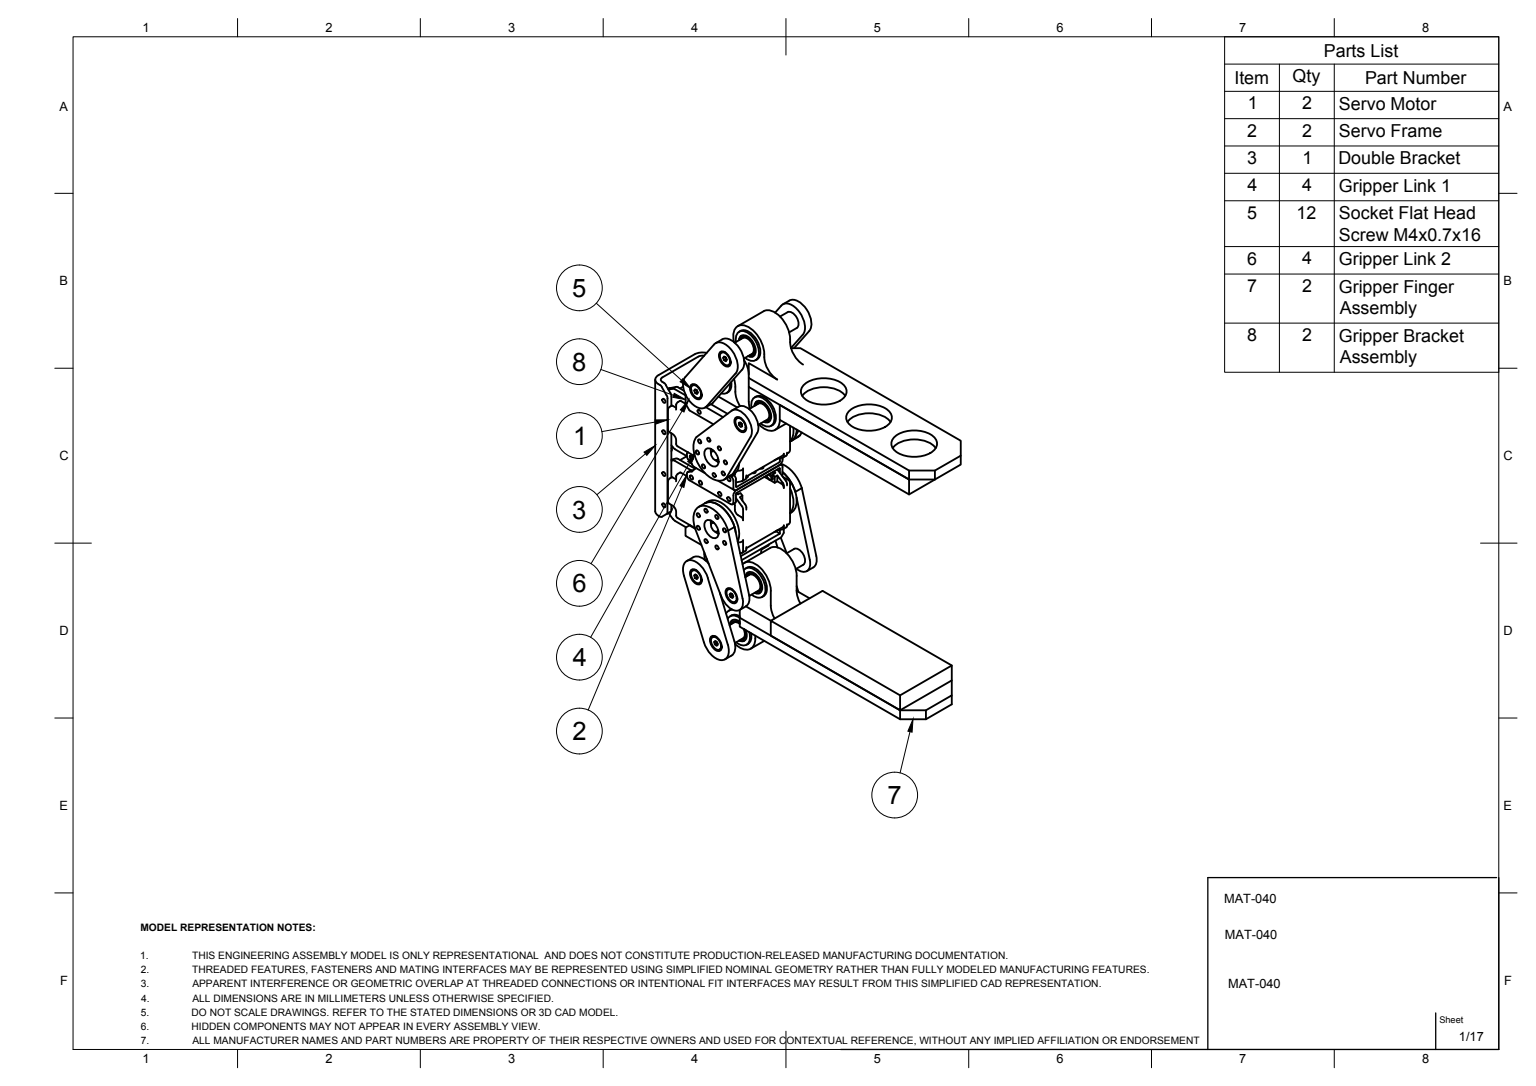
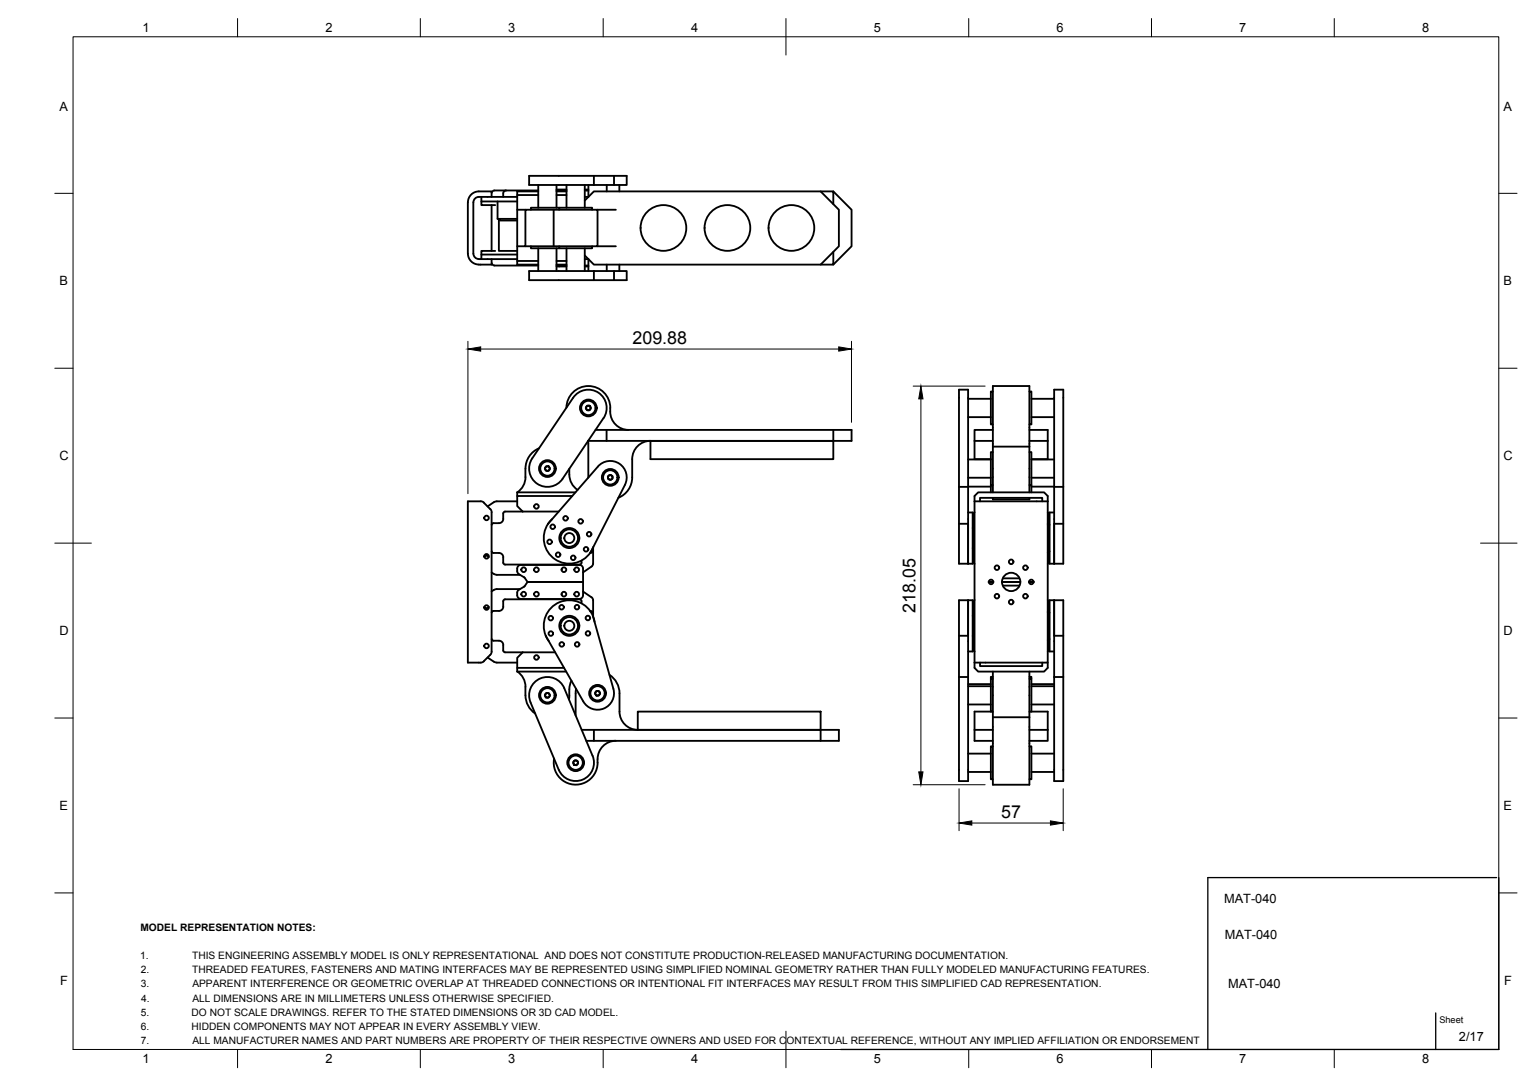
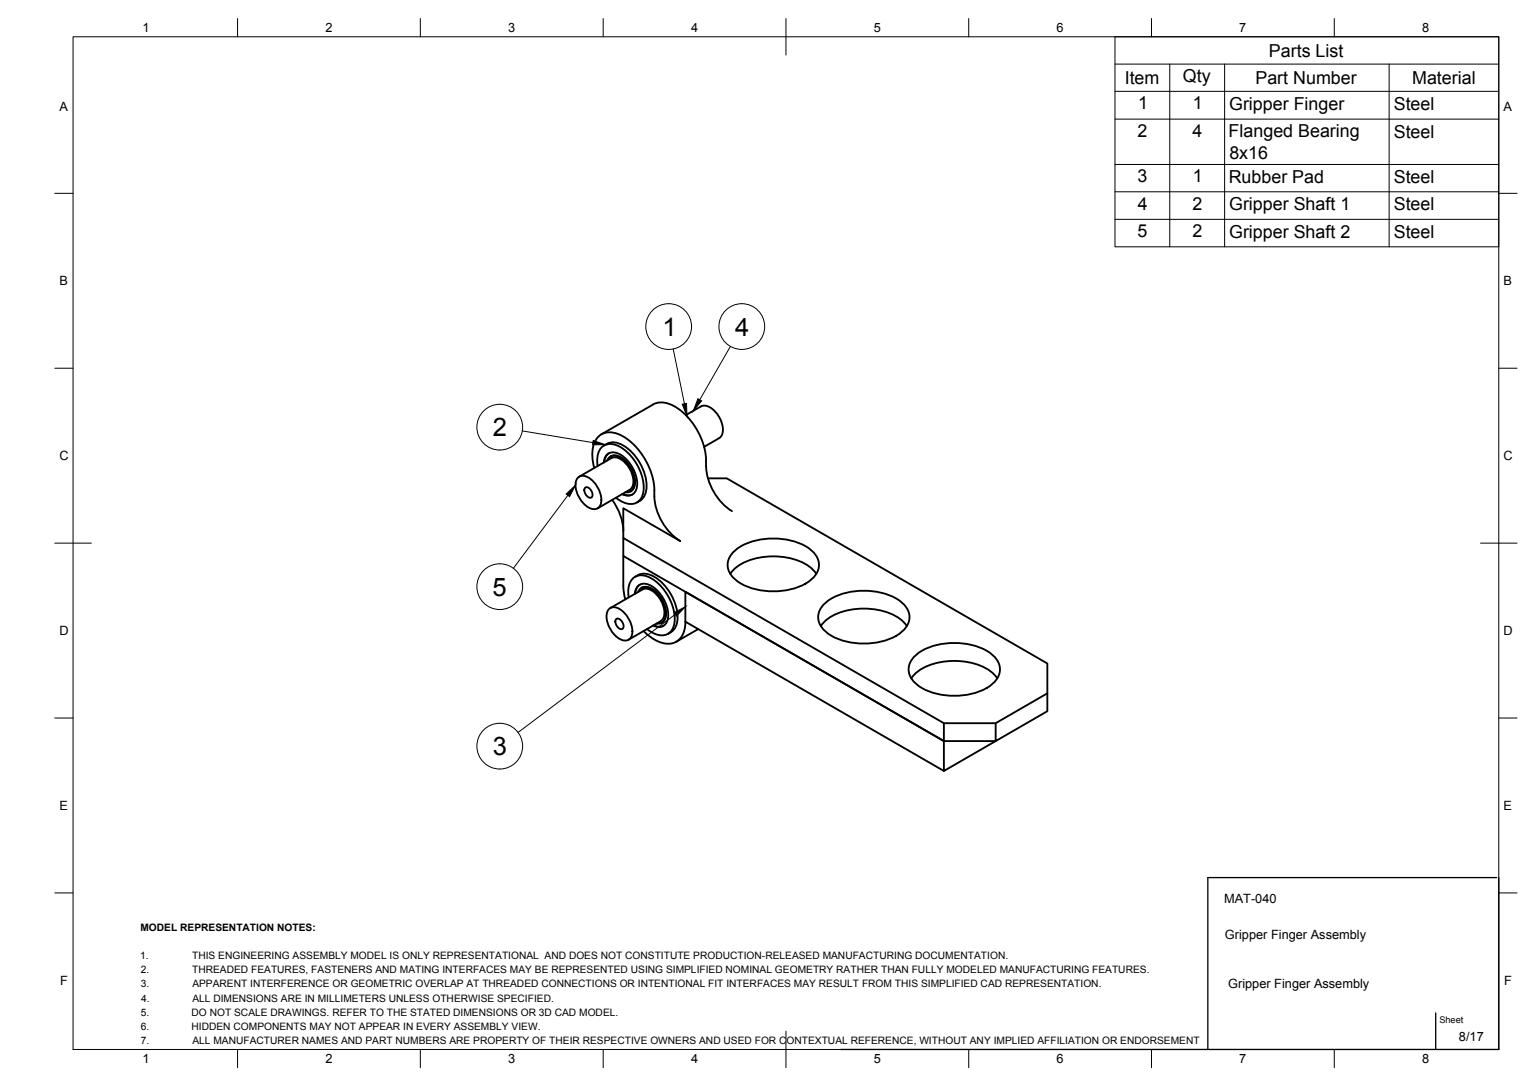
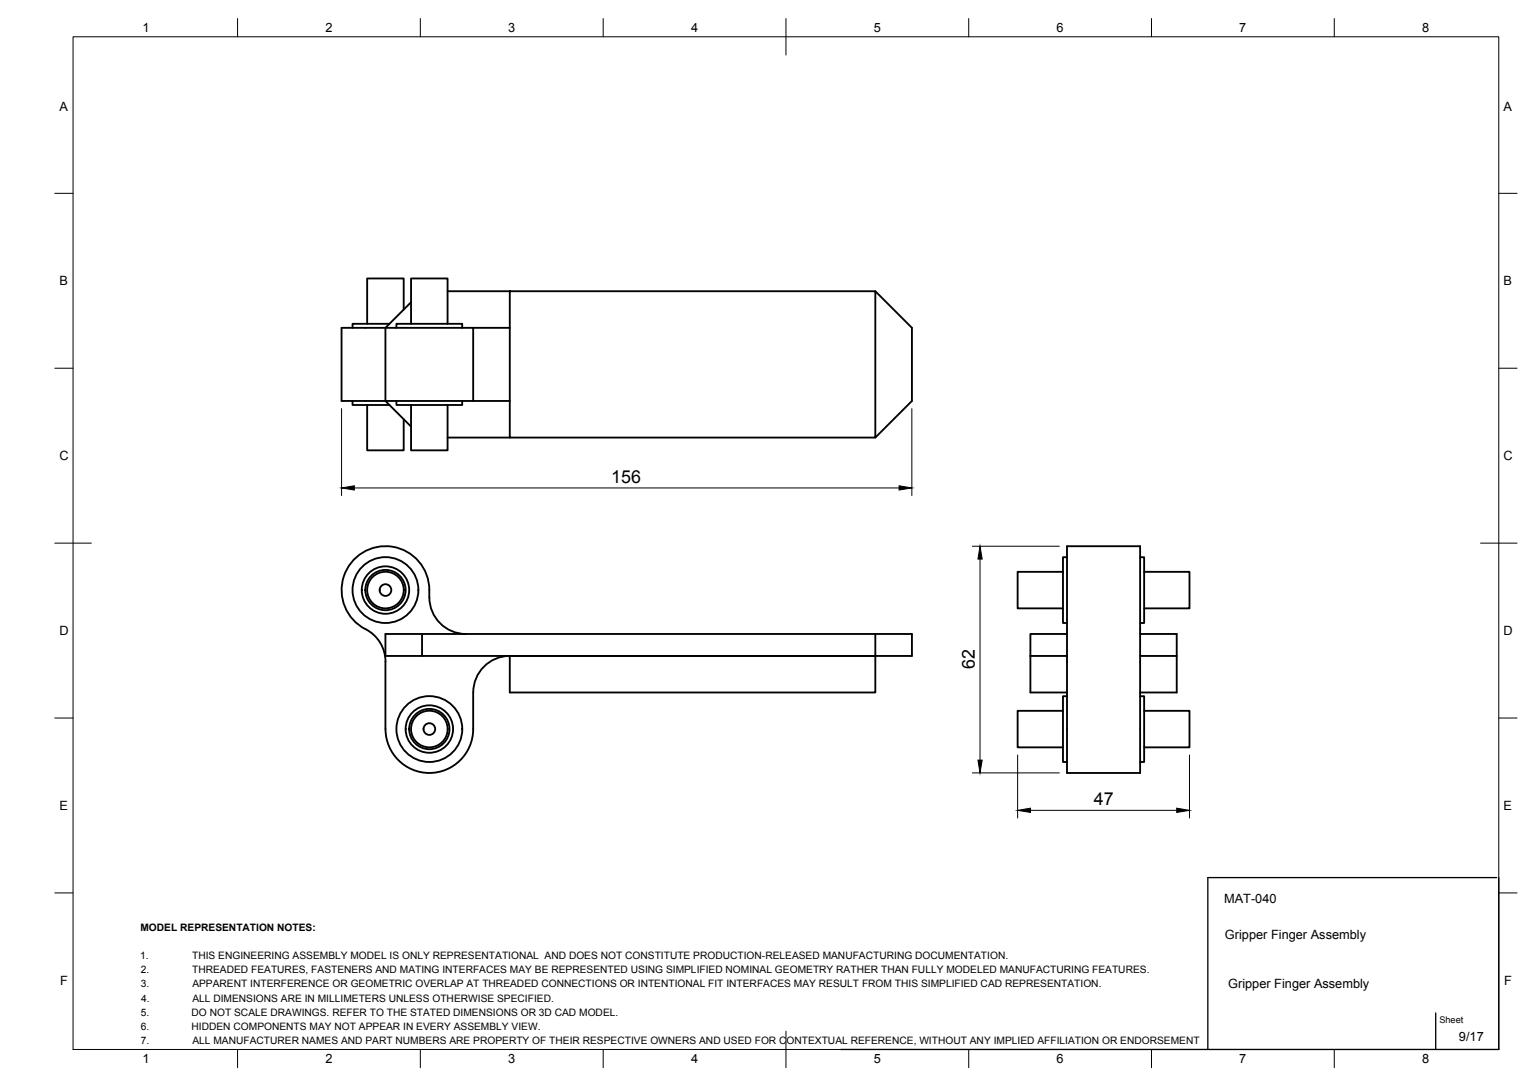
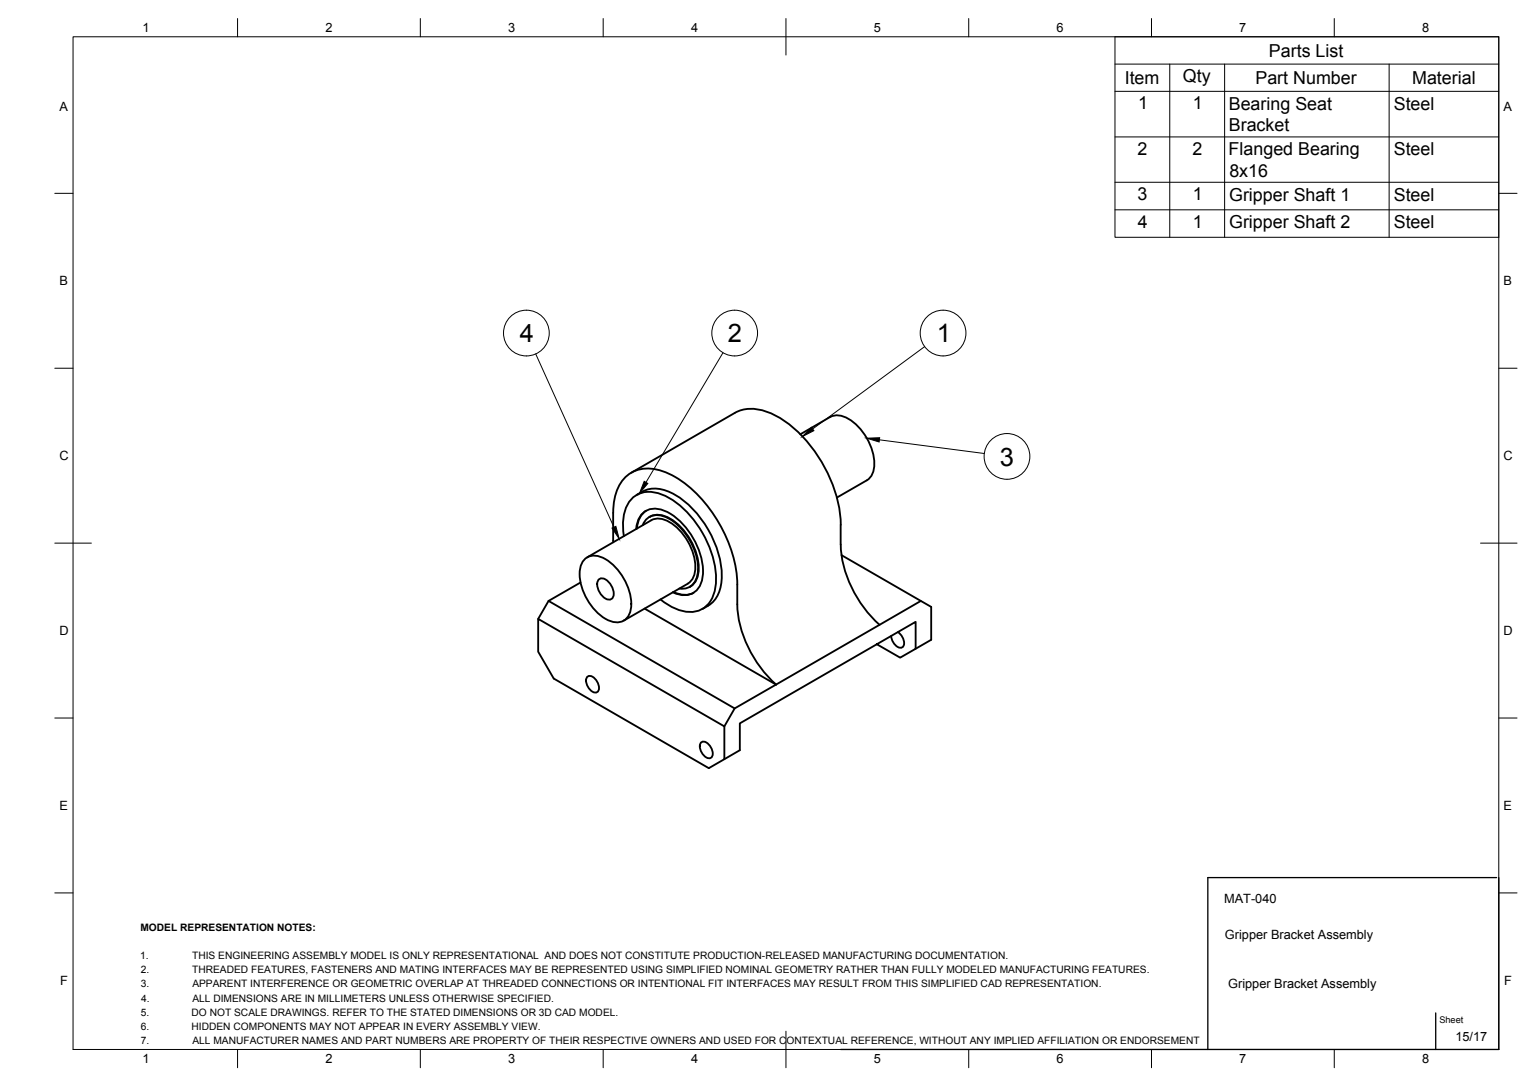
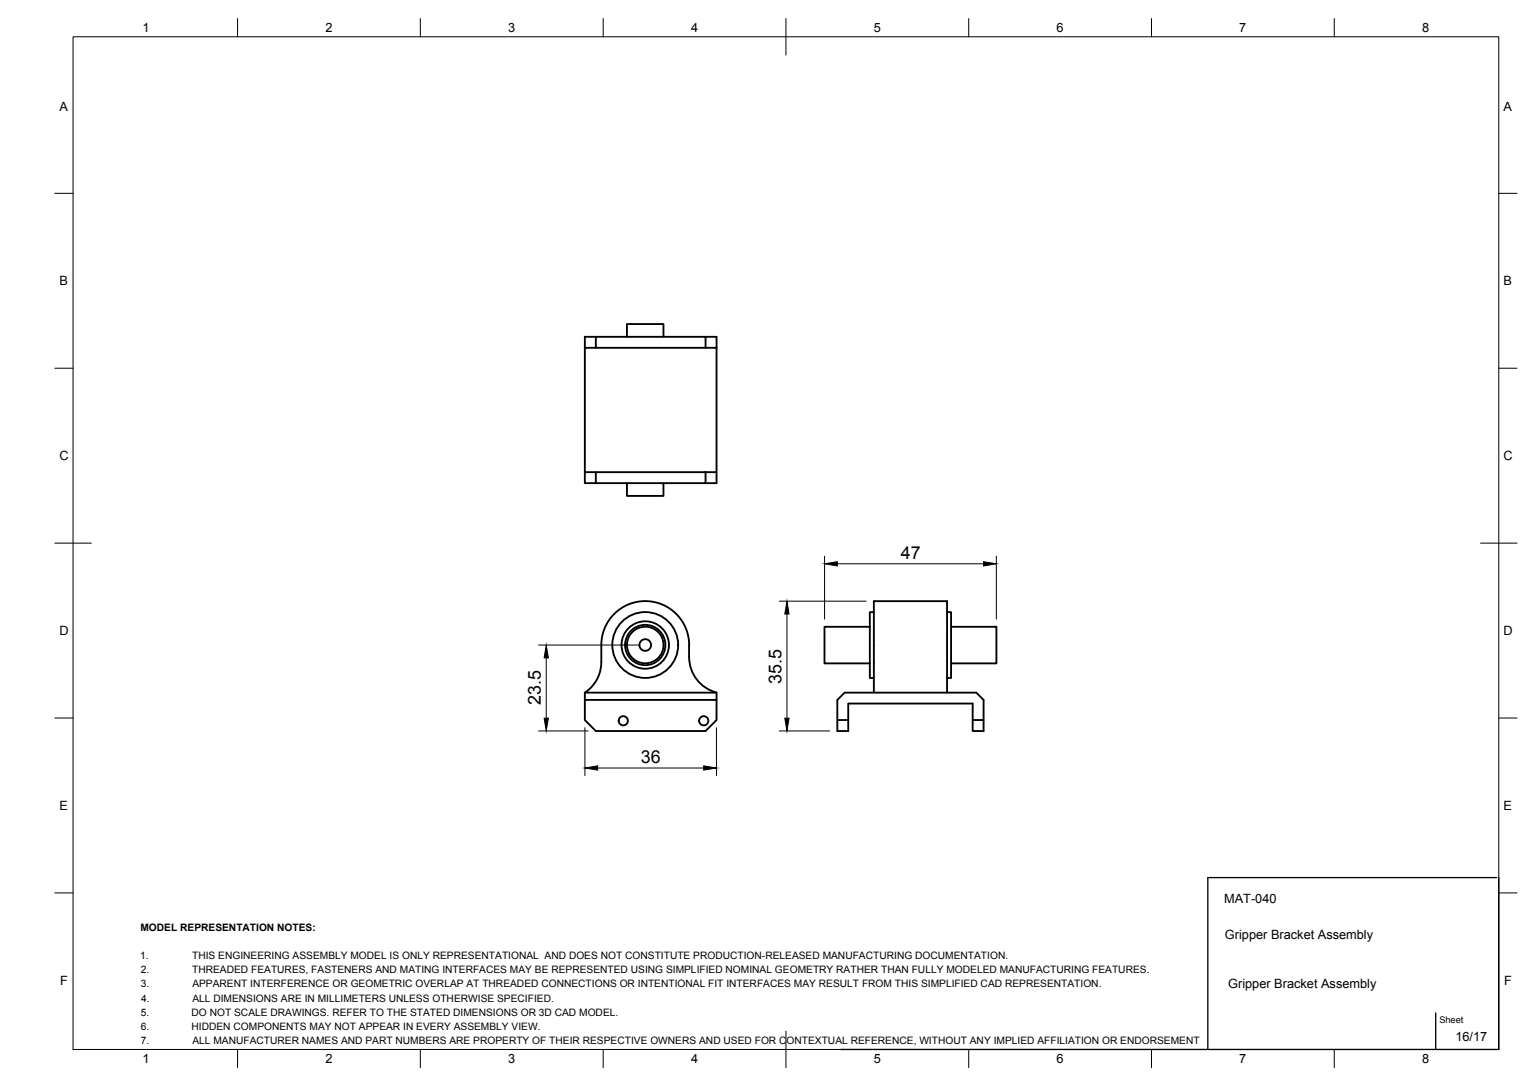
ISO-10303-21;
HEADER;
/* Generated by software containing ST-Developer
 * from STEP Tools, Inc. (www.steptools.com) 
 */

FILE_DESCRIPTION(
/* description */ ('STEP AP214'),
/* implementation_level */ '2;1');

FILE_NAME(
/* name */ 'MAT-040.step',
/* time_stamp */ '2026-11-14T21:53:28-08:00',
/* author */ (''),
/* organization */ (''),
/* preprocessor_version */ 'ST-DEVELOPER v20.2',
/* originating_system */ 'Autodesk Translation Framework v15.17.0.0',
/* authorisation */ '');

FILE_SCHEMA (('AUTOMOTIVE_DESIGN { 1 0 10303 214 3 1 1 }'));
ENDSEC;

DATA;
#10=MECHANICAL_DESIGN_GEOMETRIC_PRESENTATION_REPRESENTATION('',(#318,#319,
#320,#321,#322,#323,#324,#325,#326,#327,#328,#329,#330,#331,#332,#333,#334,
#335,#336,#337,#338,#339,#340,#341,#342,#343,#344,#345,#346,#347,#348,#349,
#350,#351,#352),#20176);
#11=ITEM_DEFINED_TRANSFORMATION($,$,#11911,#12115);
#12=ITEM_DEFINED_TRANSFORMATION($,$,#12010,#12116);
#13=ITEM_DEFINED_TRANSFORMATION($,$,#11956,#12117);
#14=ITEM_DEFINED_TRANSFORMATION($,$,#12089,#12118);
#15=ITEM_DEFINED_TRANSFORMATION($,$,#12102,#12119);
#16=ITEM_DEFINED_TRANSFORMATION($,$,#12010,#12120);
#17=ITEM_DEFINED_TRANSFORMATION($,$,#12010,#12121);
#18=ITEM_DEFINED_TRANSFORMATION($,$,#12010,#12122);
#19=ITEM_DEFINED_TRANSFORMATION($,$,#12089,#12123);
#20=ITEM_DEFINED_TRANSFORMATION($,$,#12102,#12124);
#21=ITEM_DEFINED_TRANSFORMATION($,$,#11964,#12125);
#22=ITEM_DEFINED_TRANSFORMATION($,$,#12010,#12126);
#23=ITEM_DEFINED_TRANSFORMATION($,$,#12010,#12127);
#24=ITEM_DEFINED_TRANSFORMATION($,$,#12089,#12128);
#25=ITEM_DEFINED_TRANSFORMATION($,$,#12102,#12129);
#26=ITEM_DEFINED_TRANSFORMATION($,$,#11215,#12185);
#27=ITEM_DEFINED_TRANSFORMATION($,$,#11674,#12186);
#28=ITEM_DEFINED_TRANSFORMATION($,$,#11105,#12187);
#29=ITEM_DEFINED_TRANSFORMATION($,$,#11866,#12188);
#30=ITEM_DEFINED_TRANSFORMATION($,$,#12151,#12189);
#31=ITEM_DEFINED_TRANSFORMATION($,$,#12130,#12190);
#32=ITEM_DEFINED_TRANSFORMATION($,$,#11910,#12191);
#33=ITEM_DEFINED_TRANSFORMATION($,$,#11963,#12192);
#34=ITEM_DEFINED_TRANSFORMATION($,$,#11215,#12193);
#35=ITEM_DEFINED_TRANSFORMATION($,$,#11674,#12194);
#36=ITEM_DEFINED_TRANSFORMATION($,$,#11866,#12195);
#37=ITEM_DEFINED_TRANSFORMATION($,$,#12151,#12196);
#38=ITEM_DEFINED_TRANSFORMATION($,$,#12151,#12197);
#39=ITEM_DEFINED_TRANSFORMATION($,$,#12151,#12198);
#40=ITEM_DEFINED_TRANSFORMATION($,$,#12151,#12199);
#41=ITEM_DEFINED_TRANSFORMATION($,$,#12151,#12200);
#42=ITEM_DEFINED_TRANSFORMATION($,$,#12130,#12201);
#43=ITEM_DEFINED_TRANSFORMATION($,$,#11866,#12202);
#44=ITEM_DEFINED_TRANSFORMATION($,$,#11866,#12203);
#45=ITEM_DEFINED_TRANSFORMATION($,$,#11910,#12204);
#46=ITEM_DEFINED_TRANSFORMATION($,$,#11963,#12205);
#47=ITEM_DEFINED_TRANSFORMATION($,$,#12130,#12206);
#48=ITEM_DEFINED_TRANSFORMATION($,$,#12130,#12207);
#49=ITEM_DEFINED_TRANSFORMATION($,$,#12151,#12208);
#50=ITEM_DEFINED_TRANSFORMATION($,$,#12151,#12209);
#51=ITEM_DEFINED_TRANSFORMATION($,$,#12151,#12210);
#52=ITEM_DEFINED_TRANSFORMATION($,$,#12151,#12211);
#53=ITEM_DEFINED_TRANSFORMATION($,$,#12151,#12212);
#54=ITEM_DEFINED_TRANSFORMATION($,$,#12151,#12213);
#55=(
REPRESENTATION_RELATIONSHIP($,$,#20261,#20260)
REPRESENTATION_RELATIONSHIP_WITH_TRANSFORMATION(#11)
SHAPE_REPRESENTATION_RELATIONSHIP()
);
#56=(
REPRESENTATION_RELATIONSHIP($,$,#20265,#20260)
REPRESENTATION_RELATIONSHIP_WITH_TRANSFORMATION(#12)
SHAPE_REPRESENTATION_RELATIONSHIP()
);
#57=(
REPRESENTATION_RELATIONSHIP($,$,#20262,#20260)
REPRESENTATION_RELATIONSHIP_WITH_TRANSFORMATION(#13)
SHAPE_REPRESENTATION_RELATIONSHIP()
);
#58=(
REPRESENTATION_RELATIONSHIP($,$,#20266,#20260)
REPRESENTATION_RELATIONSHIP_WITH_TRANSFORMATION(#14)
SHAPE_REPRESENTATION_RELATIONSHIP()
);
#59=(
REPRESENTATION_RELATIONSHIP($,$,#20267,#20260)
REPRESENTATION_RELATIONSHIP_WITH_TRANSFORMATION(#15)
SHAPE_REPRESENTATION_RELATIONSHIP()
);
#60=(
REPRESENTATION_RELATIONSHIP($,$,#20265,#20260)
REPRESENTATION_RELATIONSHIP_WITH_TRANSFORMATION(#16)
SHAPE_REPRESENTATION_RELATIONSHIP()
);
#61=(
REPRESENTATION_RELATIONSHIP($,$,#20265,#20260)
REPRESENTATION_RELATIONSHIP_WITH_TRANSFORMATION(#17)
SHAPE_REPRESENTATION_RELATIONSHIP()
);
#62=(
REPRESENTATION_RELATIONSHIP($,$,#20265,#20260)
REPRESENTATION_RELATIONSHIP_WITH_TRANSFORMATION(#18)
SHAPE_REPRESENTATION_RELATIONSHIP()
);
#63=(
REPRESENTATION_RELATIONSHIP($,$,#20266,#20260)
REPRESENTATION_RELATIONSHIP_WITH_TRANSFORMATION(#19)
SHAPE_REPRESENTATION_RELATIONSHIP()
);
#64=(
REPRESENTATION_RELATIONSHIP($,$,#20267,#20260)
REPRESENTATION_RELATIONSHIP_WITH_TRANSFORMATION(#20)
SHAPE_REPRESENTATION_RELATIONSHIP()
);
#65=(
REPRESENTATION_RELATIONSHIP($,$,#20264,#20263)
REPRESENTATION_RELATIONSHIP_WITH_TRANSFORMATION(#21)
SHAPE_REPRESENTATION_RELATIONSHIP()
);
#66=(
REPRESENTATION_RELATIONSHIP($,$,#20265,#20263)
REPRESENTATION_RELATIONSHIP_WITH_TRANSFORMATION(#22)
SHAPE_REPRESENTATION_RELATIONSHIP()
);
#67=(
REPRESENTATION_RELATIONSHIP($,$,#20265,#20263)
REPRESENTATION_RELATIONSHIP_WITH_TRANSFORMATION(#23)
SHAPE_REPRESENTATION_RELATIONSHIP()
);
#68=(
REPRESENTATION_RELATIONSHIP($,$,#20266,#20263)
REPRESENTATION_RELATIONSHIP_WITH_TRANSFORMATION(#24)
SHAPE_REPRESENTATION_RELATIONSHIP()
);
#69=(
REPRESENTATION_RELATIONSHIP($,$,#20267,#20263)
REPRESENTATION_RELATIONSHIP_WITH_TRANSFORMATION(#25)
SHAPE_REPRESENTATION_RELATIONSHIP()
);
#70=(
REPRESENTATION_RELATIONSHIP($,$,#20257,#20255)
REPRESENTATION_RELATIONSHIP_WITH_TRANSFORMATION(#26)
SHAPE_REPRESENTATION_RELATIONSHIP()
);
#71=(
REPRESENTATION_RELATIONSHIP($,$,#20258,#20255)
REPRESENTATION_RELATIONSHIP_WITH_TRANSFORMATION(#27)
SHAPE_REPRESENTATION_RELATIONSHIP()
);
#72=(
REPRESENTATION_RELATIONSHIP($,$,#20256,#20255)
REPRESENTATION_RELATIONSHIP_WITH_TRANSFORMATION(#28)
SHAPE_REPRESENTATION_RELATIONSHIP()
);
#73=(
REPRESENTATION_RELATIONSHIP($,$,#20259,#20255)
REPRESENTATION_RELATIONSHIP_WITH_TRANSFORMATION(#29)
SHAPE_REPRESENTATION_RELATIONSHIP()
);
#74=(
REPRESENTATION_RELATIONSHIP($,$,#20269,#20255)
REPRESENTATION_RELATIONSHIP_WITH_TRANSFORMATION(#30)
SHAPE_REPRESENTATION_RELATIONSHIP()
);
#75=(
REPRESENTATION_RELATIONSHIP($,$,#20268,#20255)
REPRESENTATION_RELATIONSHIP_WITH_TRANSFORMATION(#31)
SHAPE_REPRESENTATION_RELATIONSHIP()
);
#76=(
REPRESENTATION_RELATIONSHIP($,$,#20260,#20255)
REPRESENTATION_RELATIONSHIP_WITH_TRANSFORMATION(#32)
SHAPE_REPRESENTATION_RELATIONSHIP()
);
#77=(
REPRESENTATION_RELATIONSHIP($,$,#20263,#20255)
REPRESENTATION_RELATIONSHIP_WITH_TRANSFORMATION(#33)
SHAPE_REPRESENTATION_RELATIONSHIP()
);
#78=(
REPRESENTATION_RELATIONSHIP($,$,#20257,#20255)
REPRESENTATION_RELATIONSHIP_WITH_TRANSFORMATION(#34)
SHAPE_REPRESENTATION_RELATIONSHIP()
);
#79=(
REPRESENTATION_RELATIONSHIP($,$,#20258,#20255)
REPRESENTATION_RELATIONSHIP_WITH_TRANSFORMATION(#35)
SHAPE_REPRESENTATION_RELATIONSHIP()
);
#80=(
REPRESENTATION_RELATIONSHIP($,$,#20259,#20255)
REPRESENTATION_RELATIONSHIP_WITH_TRANSFORMATION(#36)
SHAPE_REPRESENTATION_RELATIONSHIP()
);
#81=(
REPRESENTATION_RELATIONSHIP($,$,#20269,#20255)
REPRESENTATION_RELATIONSHIP_WITH_TRANSFORMATION(#37)
SHAPE_REPRESENTATION_RELATIONSHIP()
);
#82=(
REPRESENTATION_RELATIONSHIP($,$,#20269,#20255)
REPRESENTATION_RELATIONSHIP_WITH_TRANSFORMATION(#38)
SHAPE_REPRESENTATION_RELATIONSHIP()
);
#83=(
REPRESENTATION_RELATIONSHIP($,$,#20269,#20255)
REPRESENTATION_RELATIONSHIP_WITH_TRANSFORMATION(#39)
SHAPE_REPRESENTATION_RELATIONSHIP()
);
#84=(
REPRESENTATION_RELATIONSHIP($,$,#20269,#20255)
REPRESENTATION_RELATIONSHIP_WITH_TRANSFORMATION(#40)
SHAPE_REPRESENTATION_RELATIONSHIP()
);
#85=(
REPRESENTATION_RELATIONSHIP($,$,#20269,#20255)
REPRESENTATION_RELATIONSHIP_WITH_TRANSFORMATION(#41)
SHAPE_REPRESENTATION_RELATIONSHIP()
);
#86=(
REPRESENTATION_RELATIONSHIP($,$,#20268,#20255)
REPRESENTATION_RELATIONSHIP_WITH_TRANSFORMATION(#42)
SHAPE_REPRESENTATION_RELATIONSHIP()
);
#87=(
REPRESENTATION_RELATIONSHIP($,$,#20259,#20255)
REPRESENTATION_RELATIONSHIP_WITH_TRANSFORMATION(#43)
SHAPE_REPRESENTATION_RELATIONSHIP()
);
#88=(
REPRESENTATION_RELATIONSHIP($,$,#20259,#20255)
REPRESENTATION_RELATIONSHIP_WITH_TRANSFORMATION(#44)
SHAPE_REPRESENTATION_RELATIONSHIP()
);
#89=(
REPRESENTATION_RELATIONSHIP($,$,#20260,#20255)
REPRESENTATION_RELATIONSHIP_WITH_TRANSFORMATION(#45)
SHAPE_REPRESENTATION_RELATIONSHIP()
);
#90=(
REPRESENTATION_RELATIONSHIP($,$,#20263,#20255)
REPRESENTATION_RELATIONSHIP_WITH_TRANSFORMATION(#46)
SHAPE_REPRESENTATION_RELATIONSHIP()
);
#91=(
REPRESENTATION_RELATIONSHIP($,$,#20268,#20255)
REPRESENTATION_RELATIONSHIP_WITH_TRANSFORMATION(#47)
SHAPE_REPRESENTATION_RELATIONSHIP()
);
#92=(
REPRESENTATION_RELATIONSHIP($,$,#20268,#20255)
REPRESENTATION_RELATIONSHIP_WITH_TRANSFORMATION(#48)
SHAPE_REPRESENTATION_RELATIONSHIP()
);
#93=(
REPRESENTATION_RELATIONSHIP($,$,#20269,#20255)
REPRESENTATION_RELATIONSHIP_WITH_TRANSFORMATION(#49)
SHAPE_REPRESENTATION_RELATIONSHIP()
);
#94=(
REPRESENTATION_RELATIONSHIP($,$,#20269,#20255)
REPRESENTATION_RELATIONSHIP_WITH_TRANSFORMATION(#50)
SHAPE_REPRESENTATION_RELATIONSHIP()
);
#95=(
REPRESENTATION_RELATIONSHIP($,$,#20269,#20255)
REPRESENTATION_RELATIONSHIP_WITH_TRANSFORMATION(#51)
SHAPE_REPRESENTATION_RELATIONSHIP()
);
#96=(
REPRESENTATION_RELATIONSHIP($,$,#20269,#20255)
REPRESENTATION_RELATIONSHIP_WITH_TRANSFORMATION(#52)
SHAPE_REPRESENTATION_RELATIONSHIP()
);
#97=(
REPRESENTATION_RELATIONSHIP($,$,#20269,#20255)
REPRESENTATION_RELATIONSHIP_WITH_TRANSFORMATION(#53)
SHAPE_REPRESENTATION_RELATIONSHIP()
);
#98=(
REPRESENTATION_RELATIONSHIP($,$,#20269,#20255)
REPRESENTATION_RELATIONSHIP_WITH_TRANSFORMATION(#54)
SHAPE_REPRESENTATION_RELATIONSHIP()
);
#99=CONTEXT_DEPENDENT_SHAPE_REPRESENTATION(#55,#20209);
#100=CONTEXT_DEPENDENT_SHAPE_REPRESENTATION(#56,#20210);
#101=CONTEXT_DEPENDENT_SHAPE_REPRESENTATION(#57,#20211);
#102=CONTEXT_DEPENDENT_SHAPE_REPRESENTATION(#58,#20212);
#103=CONTEXT_DEPENDENT_SHAPE_REPRESENTATION(#59,#20213);
#104=CONTEXT_DEPENDENT_SHAPE_REPRESENTATION(#60,#20214);
#105=CONTEXT_DEPENDENT_SHAPE_REPRESENTATION(#61,#20215);
#106=CONTEXT_DEPENDENT_SHAPE_REPRESENTATION(#62,#20216);
#107=CONTEXT_DEPENDENT_SHAPE_REPRESENTATION(#63,#20217);
#108=CONTEXT_DEPENDENT_SHAPE_REPRESENTATION(#64,#20218);
#109=CONTEXT_DEPENDENT_SHAPE_REPRESENTATION(#65,#20219);
#110=CONTEXT_DEPENDENT_SHAPE_REPRESENTATION(#66,#20220);
#111=CONTEXT_DEPENDENT_SHAPE_REPRESENTATION(#67,#20221);
#112=CONTEXT_DEPENDENT_SHAPE_REPRESENTATION(#68,#20222);
#113=CONTEXT_DEPENDENT_SHAPE_REPRESENTATION(#69,#20223);
#114=CONTEXT_DEPENDENT_SHAPE_REPRESENTATION(#70,#20226);
#115=CONTEXT_DEPENDENT_SHAPE_REPRESENTATION(#71,#20227);
#116=CONTEXT_DEPENDENT_SHAPE_REPRESENTATION(#72,#20228);
#117=CONTEXT_DEPENDENT_SHAPE_REPRESENTATION(#73,#20229);
#118=CONTEXT_DEPENDENT_SHAPE_REPRESENTATION(#74,#20230);
#119=CONTEXT_DEPENDENT_SHAPE_REPRESENTATION(#75,#20231);
#120=CONTEXT_DEPENDENT_SHAPE_REPRESENTATION(#76,#20232);
#121=CONTEXT_DEPENDENT_SHAPE_REPRESENTATION(#77,#20233);
#122=CONTEXT_DEPENDENT_SHAPE_REPRESENTATION(#78,#20234);
#123=CONTEXT_DEPENDENT_SHAPE_REPRESENTATION(#79,#20235);
#124=CONTEXT_DEPENDENT_SHAPE_REPRESENTATION(#80,#20236);
#125=CONTEXT_DEPENDENT_SHAPE_REPRESENTATION(#81,#20237);
#126=CONTEXT_DEPENDENT_SHAPE_REPRESENTATION(#82,#20238);
#127=CONTEXT_DEPENDENT_SHAPE_REPRESENTATION(#83,#20239);
#128=CONTEXT_DEPENDENT_SHAPE_REPRESENTATION(#84,#20240);
#129=CONTEXT_DEPENDENT_SHAPE_REPRESENTATION(#85,#20241);
#130=CONTEXT_DEPENDENT_SHAPE_REPRESENTATION(#86,#20242);
#131=CONTEXT_DEPENDENT_SHAPE_REPRESENTATION(#87,#20243);
#132=CONTEXT_DEPENDENT_SHAPE_REPRESENTATION(#88,#20244);
#133=CONTEXT_DEPENDENT_SHAPE_REPRESENTATION(#89,#20245);
#134=CONTEXT_DEPENDENT_SHAPE_REPRESENTATION(#90,#20246);
#135=CONTEXT_DEPENDENT_SHAPE_REPRESENTATION(#91,#20247);
#136=CONTEXT_DEPENDENT_SHAPE_REPRESENTATION(#92,#20248);
#137=CONTEXT_DEPENDENT_SHAPE_REPRESENTATION(#93,#20249);
#138=CONTEXT_DEPENDENT_SHAPE_REPRESENTATION(#94,#20250);
#139=CONTEXT_DEPENDENT_SHAPE_REPRESENTATION(#95,#20251);
#140=CONTEXT_DEPENDENT_SHAPE_REPRESENTATION(#96,#20252);
#141=CONTEXT_DEPENDENT_SHAPE_REPRESENTATION(#97,#20253);
#142=CONTEXT_DEPENDENT_SHAPE_REPRESENTATION(#98,#20254);
#143=NEXT_ASSEMBLY_USAGE_OCCURRENCE('Gripper Finger:1',
'Gripper Finger:1','Gripper Finger:1',#20276,#20277,'Gripper Finger:1');
#144=NEXT_ASSEMBLY_USAGE_OCCURRENCE('Flanged Bearing 8x16:1',
'Flanged Bearing 8x16:1','Flanged Bearing 8x16:1',#20276,#20281,
'Flanged Bearing 8x16:1');
#145=NEXT_ASSEMBLY_USAGE_OCCURRENCE('Rubber Pad:1','Rubber Pad:1',
'Rubber Pad:1',#20276,#20278,'Rubber Pad:1');
#146=NEXT_ASSEMBLY_USAGE_OCCURRENCE('Gripper Shaft 1:1',
'Gripper Shaft 1:1','Gripper Shaft 1:1',#20276,#20282,
'Gripper Shaft 1:1');
#147=NEXT_ASSEMBLY_USAGE_OCCURRENCE('Gripper Shaft 2:1',
'Gripper Shaft 2:1','Gripper Shaft 2:1',#20276,#20283,
'Gripper Shaft 2:1');
#148=NEXT_ASSEMBLY_USAGE_OCCURRENCE('Flanged Bearing 8x16:2',
'Flanged Bearing 8x16:2','Flanged Bearing 8x16:2',#20276,#20281,
'Flanged Bearing 8x16:2');
#149=NEXT_ASSEMBLY_USAGE_OCCURRENCE('Flanged Bearing 8x16:3',
'Flanged Bearing 8x16:3','Flanged Bearing 8x16:3',#20276,#20281,
'Flanged Bearing 8x16:3');
#150=NEXT_ASSEMBLY_USAGE_OCCURRENCE('Flanged Bearing 8x16:4',
'Flanged Bearing 8x16:4','Flanged Bearing 8x16:4',#20276,#20281,
'Flanged Bearing 8x16:4');
#151=NEXT_ASSEMBLY_USAGE_OCCURRENCE('Gripper Shaft 1:2',
'Gripper Shaft 1:2','Gripper Shaft 1:2',#20276,#20282,
'Gripper Shaft 1:2');
#152=NEXT_ASSEMBLY_USAGE_OCCURRENCE('Gripper Shaft 2:2',
'Gripper Shaft 2:2','Gripper Shaft 2:2',#20276,#20283,
'Gripper Shaft 2:2');
#153=NEXT_ASSEMBLY_USAGE_OCCURRENCE('Bearing Seat Bracket:1',
'Bearing Seat Bracket:1','Bearing Seat Bracket:1',#20279,#20280,
'Bearing Seat Bracket:1');
#154=NEXT_ASSEMBLY_USAGE_OCCURRENCE('Flanged Bearing 8x16:5',
'Flanged Bearing 8x16:5','Flanged Bearing 8x16:5',#20279,#20281,
'Flanged Bearing 8x16:5');
#155=NEXT_ASSEMBLY_USAGE_OCCURRENCE('Flanged Bearing 8x16:6',
'Flanged Bearing 8x16:6','Flanged Bearing 8x16:6',#20279,#20281,
'Flanged Bearing 8x16:6');
#156=NEXT_ASSEMBLY_USAGE_OCCURRENCE('Gripper Shaft 1:3',
'Gripper Shaft 1:3','Gripper Shaft 1:3',#20279,#20282,
'Gripper Shaft 1:3');
#157=NEXT_ASSEMBLY_USAGE_OCCURRENCE('Gripper Shaft 2:3',
'Gripper Shaft 2:3','Gripper Shaft 2:3',#20279,#20283,
'Gripper Shaft 2:3');
#158=NEXT_ASSEMBLY_USAGE_OCCURRENCE('Servo Motor:1','Servo Motor:1',
'Servo Motor:1',#20271,#20273,'Servo Motor:1');
#159=NEXT_ASSEMBLY_USAGE_OCCURRENCE('Servo Frame:1','Servo Frame:1',
'Servo Frame:1',#20271,#20274,'Servo Frame:1');
#160=NEXT_ASSEMBLY_USAGE_OCCURRENCE('Double Bracket:1',
'Double Bracket:1','Double Bracket:1',#20271,#20272,'Double Bracket:1');
#161=NEXT_ASSEMBLY_USAGE_OCCURRENCE('Gripper Link 1:1',
'Gripper Link 1:1','Gripper Link 1:1',#20271,#20275,'Gripper Link 1:1');
#162=NEXT_ASSEMBLY_USAGE_OCCURRENCE(
'Socket Flat Head Screw M4x0.7x16:1',
'Socket Flat Head Screw M4x0.7x16:1',
'Socket Flat Head Screw M4x0.7x16:1',#20271,#20285,
'Socket Flat Head Screw M4x0.7x16:1');
#163=NEXT_ASSEMBLY_USAGE_OCCURRENCE('Gripper Link 2:1',
'Gripper Link 2:1','Gripper Link 2:1',#20271,#20284,'Gripper Link 2:1');
#164=NEXT_ASSEMBLY_USAGE_OCCURRENCE('Gripper Finger Assembly:1',
'Gripper Finger Assembly:1','Gripper Finger Assembly:1',#20271,#20276,
'Gripper Finger Assembly:1');
#165=NEXT_ASSEMBLY_USAGE_OCCURRENCE('Gripper Bracket Assembly:1',
'Gripper Bracket Assembly:1','Gripper Bracket Assembly:1',#20271,#20279,
'Gripper Bracket Assembly:1');
#166=NEXT_ASSEMBLY_USAGE_OCCURRENCE('Servo Motor:2','Servo Motor:2',
'Servo Motor:2',#20271,#20273,'Servo Motor:2');
#167=NEXT_ASSEMBLY_USAGE_OCCURRENCE('Servo Frame:2','Servo Frame:2',
'Servo Frame:2',#20271,#20274,'Servo Frame:2');
#168=NEXT_ASSEMBLY_USAGE_OCCURRENCE('Gripper Link 1:2',
'Gripper Link 1:2','Gripper Link 1:2',#20271,#20275,'Gripper Link 1:2');
#169=NEXT_ASSEMBLY_USAGE_OCCURRENCE(
'Socket Flat Head Screw M4x0.7x16:2',
'Socket Flat Head Screw M4x0.7x16:2',
'Socket Flat Head Screw M4x0.7x16:2',#20271,#20285,
'Socket Flat Head Screw M4x0.7x16:2');
#170=NEXT_ASSEMBLY_USAGE_OCCURRENCE(
'Socket Flat Head Screw M4x0.7x16:3',
'Socket Flat Head Screw M4x0.7x16:3',
'Socket Flat Head Screw M4x0.7x16:3',#20271,#20285,
'Socket Flat Head Screw M4x0.7x16:3');
#171=NEXT_ASSEMBLY_USAGE_OCCURRENCE(
'Socket Flat Head Screw M4x0.7x16:4',
'Socket Flat Head Screw M4x0.7x16:4',
'Socket Flat Head Screw M4x0.7x16:4',#20271,#20285,
'Socket Flat Head Screw M4x0.7x16:4');
#172=NEXT_ASSEMBLY_USAGE_OCCURRENCE(
'Socket Flat Head Screw M4x0.7x16:5',
'Socket Flat Head Screw M4x0.7x16:5',
'Socket Flat Head Screw M4x0.7x16:5',#20271,#20285,
'Socket Flat Head Screw M4x0.7x16:5');
#173=NEXT_ASSEMBLY_USAGE_OCCURRENCE(
'Socket Flat Head Screw M4x0.7x16:6',
'Socket Flat Head Screw M4x0.7x16:6',
'Socket Flat Head Screw M4x0.7x16:6',#20271,#20285,
'Socket Flat Head Screw M4x0.7x16:6');
#174=NEXT_ASSEMBLY_USAGE_OCCURRENCE('Gripper Link 2:2',
'Gripper Link 2:2','Gripper Link 2:2',#20271,#20284,'Gripper Link 2:2');
#175=NEXT_ASSEMBLY_USAGE_OCCURRENCE('Gripper Link 1:3',
'Gripper Link 1:3','Gripper Link 1:3',#20271,#20275,'Gripper Link 1:3');
#176=NEXT_ASSEMBLY_USAGE_OCCURRENCE('Gripper Link 1:4',
'Gripper Link 1:4','Gripper Link 1:4',#20271,#20275,'Gripper Link 1:4');
#177=NEXT_ASSEMBLY_USAGE_OCCURRENCE('Gripper Finger Assembly:2',
'Gripper Finger Assembly:2','Gripper Finger Assembly:2',#20271,#20276,
'Gripper Finger Assembly:2');
#178=NEXT_ASSEMBLY_USAGE_OCCURRENCE('Gripper Bracket Assembly:2',
'Gripper Bracket Assembly:2','Gripper Bracket Assembly:2',#20271,#20279,
'Gripper Bracket Assembly:2');
#179=NEXT_ASSEMBLY_USAGE_OCCURRENCE('Gripper Link 2:3',
'Gripper Link 2:3','Gripper Link 2:3',#20271,#20284,'Gripper Link 2:3');
#180=NEXT_ASSEMBLY_USAGE_OCCURRENCE('Gripper Link 2:4',
'Gripper Link 2:4','Gripper Link 2:4',#20271,#20284,'Gripper Link 2:4');
#181=NEXT_ASSEMBLY_USAGE_OCCURRENCE(
'Socket Flat Head Screw M4x0.7x16:7',
'Socket Flat Head Screw M4x0.7x16:7',
'Socket Flat Head Screw M4x0.7x16:7',#20271,#20285,
'Socket Flat Head Screw M4x0.7x16:7');
#182=NEXT_ASSEMBLY_USAGE_OCCURRENCE(
'Socket Flat Head Screw M4x0.7x16:8',
'Socket Flat Head Screw M4x0.7x16:8',
'Socket Flat Head Screw M4x0.7x16:8',#20271,#20285,
'Socket Flat Head Screw M4x0.7x16:8');
#183=NEXT_ASSEMBLY_USAGE_OCCURRENCE(
'Socket Flat Head Screw M4x0.7x16:9',
'Socket Flat Head Screw M4x0.7x16:9',
'Socket Flat Head Screw M4x0.7x16:9',#20271,#20285,
'Socket Flat Head Screw M4x0.7x16:9');
#184=NEXT_ASSEMBLY_USAGE_OCCURRENCE(
'Socket Flat Head Screw M4x0.7x16:10',
'Socket Flat Head Screw M4x0.7x16:10',
'Socket Flat Head Screw M4x0.7x16:10',#20271,#20285,
'Socket Flat Head Screw M4x0.7x16:10');
#185=NEXT_ASSEMBLY_USAGE_OCCURRENCE(
'Socket Flat Head Screw M4x0.7x16:11',
'Socket Flat Head Screw M4x0.7x16:11',
'Socket Flat Head Screw M4x0.7x16:11',#20271,#20285,
'Socket Flat Head Screw M4x0.7x16:11');
#186=NEXT_ASSEMBLY_USAGE_OCCURRENCE(
'Socket Flat Head Screw M4x0.7x16:12',
'Socket Flat Head Screw M4x0.7x16:12',
'Socket Flat Head Screw M4x0.7x16:12',#20271,#20285,
'Socket Flat Head Screw M4x0.7x16:12');
#187=OPEN_SHELL('',(#10781));
#188=OPEN_SHELL('',(#10782));
#189=OPEN_SHELL('',(#10783));
#190=OPEN_SHELL('',(#10784));
#191=OPEN_SHELL('',(#10785));
#192=OPEN_SHELL('',(#10786));
#193=OPEN_SHELL('',(#10787));
#194=OPEN_SHELL('',(#10788));
#195=SHELL_BASED_SURFACE_MODEL('Body2',(#187));
#196=SHELL_BASED_SURFACE_MODEL('Body3',(#188));
#197=SHELL_BASED_SURFACE_MODEL('Body4',(#189));
#198=SHELL_BASED_SURFACE_MODEL('Body5',(#190));
#199=SHELL_BASED_SURFACE_MODEL('Body6',(#191));
#200=SHELL_BASED_SURFACE_MODEL('Body7',(#192));
#201=SHELL_BASED_SURFACE_MODEL('Body8',(#193));
#202=SHELL_BASED_SURFACE_MODEL('Body9',(#194));
#203=ELLIPSE('',#11797,7.14648376237048,6.18893462761436);
#204=ELLIPSE('',#11803,7.14646345436459,6.18889945302544);
#205=CONICAL_SURFACE('',#11750,1.34999999991669,0.785398163397448);
#206=CONICAL_SURFACE('',#11752,1.34999999991669,0.785398163397448);
#207=CONICAL_SURFACE('',#11754,1.34999999991669,0.785398163397448);
#208=CONICAL_SURFACE('',#11756,1.34999999991669,0.785398163397448);
#209=CONICAL_SURFACE('',#11758,1.34999999990714,0.785398163397448);
#210=CONICAL_SURFACE('',#11760,1.34999999990714,0.785398163397448);
#211=CONICAL_SURFACE('',#11762,1.34999999990714,0.785398163397448);
#212=CONICAL_SURFACE('',#11764,1.34999999990714,0.785398163397448);
#213=CONICAL_SURFACE('',#11766,5.19997115839037,0.785393345879516);
#214=CONICAL_SURFACE('',#11867,4.59,0.785398163397449);
#215=CONICAL_SURFACE('',#12015,4.25,0.785398163397453);
#216=CONICAL_SURFACE('',#12021,4.,0.785398163397443);
#217=CONICAL_SURFACE('',#12084,8.,0.785398163397446);
#218=CONICAL_SURFACE('',#12131,4.59,0.785398163397451);
#219=CONICAL_SURFACE('',#12136,4.59,0.785398163397451);
#220=CONICAL_SURFACE('',#12152,1.25,1.04719755119659);
#221=CONICAL_SURFACE('',#12166,3.9,0.785398163397451);
#222=CONICAL_SURFACE('',#12169,1.61,0.785398163397478);
#223=TOROIDAL_SURFACE('',#11390,2.00000000000006,1.49999999999999);
#224=TOROIDAL_SURFACE('',#11425,1.99999999999991,1.5);
#225=TOROIDAL_SURFACE('',#11523,3.85000000000003,1.50000000000001);
#226=TOROIDAL_SURFACE('',#11533,3.85000000000009,1.50000000000001);
#227=TOROIDAL_SURFACE('',#11543,3.85,1.5);
#228=TOROIDAL_SURFACE('',#11553,3.84999999999996,1.49999999999999);
#229=TOROIDAL_SURFACE('',#12011,6.,1.21175743903915);
#230=TOROIDAL_SURFACE('',#12075,6.,1.21175743903915);
#231=TOROIDAL_SURFACE('',#12159,2.2,0.2);
#232=B_SPLINE_SURFACE_WITH_KNOTS('',3,3,((#16443,#16444,#16445,#16446),
(#16447,#16448,#16449,#16450),(#16451,#16452,#16453,#16454),(#16455,#16456,
#16457,#16458),(#16459,#16460,#16461,#16462),(#16463,#16464,#16465,#16466),
(#16467,#16468,#16469,#16470),(#16471,#16472,#16473,#16474),(#16475,#16476,
#16477,#16478),(#16479,#16480,#16481,#16482),(#16483,#16484,#16485,#16486)),
 .UNSPECIFIED.,.F.,.F.,.F.,(4,1,1,1,1,1,1,1,4),(4,4),(-1.345105E-12,0.125,
0.25,0.375,0.5,0.625,0.75,0.875,0.999999999999432),(-0.007830111379204,
1.00000000177778),.UNSPECIFIED.);
#233=B_SPLINE_SURFACE_WITH_KNOTS('',3,3,((#16489,#16490,#16491,#16492),
(#16493,#16494,#16495,#16496),(#16497,#16498,#16499,#16500),(#16501,#16502,
#16503,#16504),(#16505,#16506,#16507,#16508),(#16509,#16510,#16511,#16512),
(#16513,#16514,#16515,#16516),(#16517,#16518,#16519,#16520),(#16521,#16522,
#16523,#16524),(#16525,#16526,#16527,#16528),(#16529,#16530,#16531,#16532)),
 .UNSPECIFIED.,.F.,.F.,.F.,(4,1,1,1,1,1,1,1,4),(4,4),(-0.000181680414011076,
0.125,0.25,0.375,0.5,0.625,0.75,0.875,1.00018168041298),(-0.007830111378265,
1.00000000177562),.UNSPECIFIED.);
#234=B_SPLINE_SURFACE_WITH_KNOTS('',3,3,((#18463,#18464,#18465,#18466),
(#18467,#18468,#18469,#18470),(#18471,#18472,#18473,#18474),(#18475,#18476,
#18477,#18478),(#18479,#18480,#18481,#18482),(#18483,#18484,#18485,#18486),
(#18487,#18488,#18489,#18490),(#18491,#18492,#18493,#18494),(#18495,#18496,
#18497,#18498),(#18499,#18500,#18501,#18502),(#18503,#18504,#18505,#18506)),
 .UNSPECIFIED.,.F.,.F.,.F.,(4,1,1,1,1,1,1,1,4),(4,4),(-0.000181679232336337,
0.125,0.25,0.375,0.5,0.625,0.75,0.875,1.00018167923146),(-0.007830111378221,
1.00000000177564),.UNSPECIFIED.);
#235=B_SPLINE_SURFACE_WITH_KNOTS('',3,3,((#18507,#18508,#18509,#18510),
(#18511,#18512,#18513,#18514),(#18515,#18516,#18517,#18518),(#18519,#18520,
#18521,#18522),(#18523,#18524,#18525,#18526),(#18527,#18528,#18529,#18530),
(#18531,#18532,#18533,#18534),(#18535,#18536,#18537,#18538),(#18539,#18540,
#18541,#18542),(#18543,#18544,#18545,#18546),(#18547,#18548,#18549,#18550)),
 .UNSPECIFIED.,.F.,.F.,.F.,(4,1,1,1,1,1,1,1,4),(4,4),(-1.346238E-12,0.125,
0.25,0.375,0.5,0.625,0.75,0.875,0.999999999999431),(-0.007830111379204,
1.00000000177778),.UNSPECIFIED.);
#236=B_SPLINE_SURFACE_WITH_KNOTS('',3,3,((#18551,#18552,#18553,#18554),
(#18555,#18556,#18557,#18558),(#18559,#18560,#18561,#18562),(#18563,#18564,
#18565,#18566),(#18567,#18568,#18569,#18570),(#18571,#18572,#18573,#18574),
(#18575,#18576,#18577,#18578),(#18579,#18580,#18581,#18582),(#18583,#18584,
#18585,#18586),(#18587,#18588,#18589,#18590),(#18591,#18592,#18593,#18594)),
 .UNSPECIFIED.,.F.,.F.,.F.,(4,1,1,1,1,1,1,1,4),(4,4),(-1.340881E-12,0.125,
0.25,0.375,0.5,0.625,0.75,0.875,0.999999999999857),(-0.007830111378128,
1.00000000177777),.UNSPECIFIED.);
#237=B_SPLINE_SURFACE_WITH_KNOTS('',3,3,((#18595,#18596,#18597,#18598),
(#18599,#18600,#18601,#18602),(#18603,#18604,#18605,#18606),(#18607,#18608,
#18609,#18610),(#18611,#18612,#18613,#18614),(#18615,#18616,#18617,#18618),
(#18619,#18620,#18621,#18622),(#18623,#18624,#18625,#18626),(#18627,#18628,
#18629,#18630),(#18631,#18632,#18633,#18634),(#18635,#18636,#18637,#18638)),
 .UNSPECIFIED.,.F.,.F.,.F.,(4,1,1,1,1,1,1,1,4),(4,4),(-0.000181679230988105,
0.125,0.25,0.375,0.5,0.625,0.75,0.875,1.00018167923038),(-0.007830111380071,
1.00000000177566),.UNSPECIFIED.);
#238=B_SPLINE_SURFACE_WITH_KNOTS('',3,3,((#18639,#18640,#18641,#18642),
(#18643,#18644,#18645,#18646),(#18647,#18648,#18649,#18650),(#18651,#18652,
#18653,#18654),(#18655,#18656,#18657,#18658),(#18659,#18660,#18661,#18662),
(#18663,#18664,#18665,#18666),(#18667,#18668,#18669,#18670),(#18671,#18672,
#18673,#18674),(#18675,#18676,#18677,#18678),(#18679,#18680,#18681,#18682)),
 .UNSPECIFIED.,.F.,.F.,.F.,(4,1,1,1,1,1,1,1,4),(4,4),(-0.000181679231834029,
0.125,0.25,0.375,0.5,0.625,0.75,0.875,1.0001816792308),(-0.00783011137814,
1.00000000177563),.UNSPECIFIED.);
#239=B_SPLINE_SURFACE_WITH_KNOTS('',3,3,((#18683,#18684,#18685,#18686),
(#18687,#18688,#18689,#18690),(#18691,#18692,#18693,#18694),(#18695,#18696,
#18697,#18698),(#18699,#18700,#18701,#18702),(#18703,#18704,#18705,#18706),
(#18707,#18708,#18709,#18710),(#18711,#18712,#18713,#18714),(#18715,#18716,
#18717,#18718),(#18719,#18720,#18721,#18722),(#18723,#18724,#18725,#18726)),
 .UNSPECIFIED.,.F.,.F.,.F.,(4,1,1,1,1,1,1,1,4),(4,4),(-4.869438E-14,0.125,
0.25,0.375,0.5,0.625,0.75,0.875,0.999999999999432),(-0.007830111379894,
1.00000000177778),.UNSPECIFIED.);
#240=B_SPLINE_SURFACE_WITH_KNOTS('',3,3,((#19092,#19093,#19094,#19095),
(#19096,#19097,#19098,#19099),(#19100,#19101,#19102,#19103),(#19104,#19105,
#19106,#19107),(#19108,#19109,#19110,#19111),(#19112,#19113,#19114,#19115),
(#19116,#19117,#19118,#19119),(#19120,#19121,#19122,#19123),(#19124,#19125,
#19126,#19127)),.UNSPECIFIED.,.F.,.F.,.F.,(4,1,1,1,1,1,4),(4,4),(-0.01838458257717,
0.,0.25,0.5,0.75,1.,1.018710256812),(-0.03706965294501,1.037304298792),
 .UNSPECIFIED.);
#241=B_SPLINE_SURFACE_WITH_KNOTS('',3,3,((#19144,#19145,#19146,#19147),
(#19148,#19149,#19150,#19151),(#19152,#19153,#19154,#19155),(#19156,#19157,
#19158,#19159),(#19160,#19161,#19162,#19163),(#19164,#19165,#19166,#19167),
(#19168,#19169,#19170,#19171),(#19172,#19173,#19174,#19175),(#19176,#19177,
#19178,#19179)),.UNSPECIFIED.,.F.,.F.,.F.,(4,1,1,1,1,1,4),(4,4),(-0.01864501026175,
0.,0.25,0.5,0.75,1.,1.018470834436),(-0.03706965294501,1.037304298792),
 .UNSPECIFIED.);
#242=B_SPLINE_SURFACE_WITH_KNOTS('',3,3,((#19239,#19240,#19241,#19242),
(#19243,#19244,#19245,#19246),(#19247,#19248,#19249,#19250),(#19251,#19252,
#19253,#19254),(#19255,#19256,#19257,#19258),(#19259,#19260,#19261,#19262)),
 .UNSPECIFIED.,.F.,.F.,.F.,(4,1,1,4),(4,4),(-0.7776806408489,0.,1.,1.777680640849),
(-0.03706965294501,1.037069667454),.UNSPECIFIED.);
#243=B_SPLINE_SURFACE_WITH_KNOTS('',3,3,((#19263,#19264,#19265,#19266),
(#19267,#19268,#19269,#19270),(#19271,#19272,#19273,#19274),(#19275,#19276,
#19277,#19278),(#19279,#19280,#19281,#19282),(#19283,#19284,#19285,#19286)),
 .UNSPECIFIED.,.F.,.F.,.F.,(4,1,1,4),(4,4),(-0.7776806408488,0.,1.,1.777680640849),
(-0.03706965294501,1.037069667454),.UNSPECIFIED.);
#244=SPHERICAL_SURFACE('',#11302,1.5);
#245=SPHERICAL_SURFACE('',#11304,1.5);
#246=SPHERICAL_SURFACE('',#11635,1.5);
#247=SPHERICAL_SURFACE('',#11636,1.5);
#248=SPHERICAL_SURFACE('',#11637,1.5);
#249=SPHERICAL_SURFACE('',#11638,1.49999999999999);
#250=SPHERICAL_SURFACE('',#11639,1.49999999999999);
#251=SPHERICAL_SURFACE('',#11640,1.50000000000001);
#252=SPHERICAL_SURFACE('',#12029,1.21175743903915);
#253=SPHERICAL_SURFACE('',#12031,1.21175743903915);
#254=SPHERICAL_SURFACE('',#12033,1.21175743903915);
#255=SPHERICAL_SURFACE('',#12035,1.21175743903915);
#256=SPHERICAL_SURFACE('',#12037,1.21175743903915);
#257=SPHERICAL_SURFACE('',#12039,1.21175743903915);
#258=SPHERICAL_SURFACE('',#12041,1.21175743903915);
#259=SPHERICAL_SURFACE('',#12043,1.21175743903915);
#260=SPHERICAL_SURFACE('',#12045,1.21175743903915);
#261=SPHERICAL_SURFACE('',#12047,1.21175743903915);
#262=SPHERICAL_SURFACE('',#12049,1.21175743903915);
#263=SPHERICAL_SURFACE('',#12051,1.21175743903915);
#264=B_SPLINE_CURVE_WITH_KNOTS('',3,(#15932,#15933,#15934,#15935),
 .UNSPECIFIED.,.F.,.F.,(4,4),(0.,1.),.UNSPECIFIED.);
#265=B_SPLINE_CURVE_WITH_KNOTS('',3,(#15937,#15938,#15939,#15940,#15941,
#15942,#15943,#15944,#15945,#15946,#15947,#15948,#15949,#15950,#15951,#15952,
#15953,#15954,#15955,#15956,#15957,#15958,#15959,#15960,#15961,#15962,#15963,
#15964,#15965,#15966,#15967,#15968,#15969,#15970,#15971,#15972,#15973,#15974,
#15975,#15976,#15977,#15978,#15979,#15980,#15981,#15982,#15983,#15984,#15985,
#15986,#15987,#15988,#15989,#15990,#15991,#15992,#15993,#15994,#15995,#15996,
#15997,#15998,#15999,#16000,#16001,#16002,#16003,#16004,#16005,#16006,#16007,
#16008,#16009,#16010,#16011,#16012,#16013,#16014,#16015,#16016,#16017,#16018,
#16019,#16020,#16021,#16022,#16023,#16024,#16025,#16026,#16027,#16028,#16029,
#16030,#16031,#16032,#16033,#16034,#16035,#16036,#16037,#16038,#16039,#16040,
#16041,#16042,#16043,#16044,#16045,#16046,#16047,#16048,#16049,#16050,#16051,
#16052,#16053,#16054,#16055,#16056,#16057,#16058,#16059,#16060,#16061,#16062,
#16063,#16064,#16065,#16066,#16067,#16068,#16069,#16070,#16071,#16072,#16073,
#16074,#16075,#16076,#16077,#16078,#16079,#16080,#16081,#16082,#16083,#16084,
#16085,#16086,#16087,#16088,#16089,#16090,#16091,#16092,#16093,#16094,#16095,
#16096,#16097,#16098,#16099,#16100,#16101,#16102,#16103,#16104,#16105,#16106,
#16107,#16108,#16109,#16110,#16111,#16112,#16113,#16114,#16115,#16116,#16117),
 .UNSPECIFIED.,.F.,.F.,(4,3,3,3,3,3,3,3,3,3,3,3,3,3,3,3,3,3,3,3,3,3,3,3,
3,3,3,3,3,3,3,3,3,3,3,3,3,3,3,3,3,3,3,3,3,3,3,3,3,3,3,3,3,3,3,3,3,3,3,3,
4),(0.,0.0533325059244852,0.0625000000000259,0.0841085084394197,0.105548099870102,
0.125000000000052,0.17630092547594,0.187500000000078,0.218750000000089,
0.234375000000094,0.242187500000095,0.24754815261247,0.250000000000095,
0.287437188888397,0.323763744374451,0.36001030828085,0.393976204362633,
0.427224027426155,0.459537106534552,0.468750000000046,0.484375000000039,
0.492187500000034,0.496093750000031,0.499047272546838,0.500000000000028,
0.531406909119804,0.562578454559912,0.59375000000002,0.605659576286838,
0.617496842340772,0.625000000000018,0.661169076078725,0.687500000000014,
0.71875000000001,0.73437500000001,0.742187500000009,0.750000000000009,0.781516758419965,
0.812499999999997,0.832471681794437,0.852007987221176,0.870840274034354,
0.874999999999985,0.897518269248034,0.906249999999981,0.921874999999979,
0.92968749999998,0.934543491568822,0.93749999999998,0.950765500153561,0.963898282500585,
0.968749999999992,0.97863369201704,0.984374999999997,0.991614704653795,
0.992187500000001,0.994140625,0.995507742631974,0.99609375,0.998075415265071,
1.),.UNSPECIFIED.);
#266=B_SPLINE_CURVE_WITH_KNOTS('',3,(#16122,#16123,#16124,#16125,#16126,
#16127,#16128,#16129,#16130,#16131,#16132,#16133,#16134,#16135,#16136,#16137,
#16138,#16139,#16140,#16141,#16142,#16143,#16144,#16145,#16146,#16147,#16148,
#16149,#16150,#16151,#16152,#16153,#16154,#16155,#16156,#16157,#16158,#16159,
#16160,#16161,#16162,#16163,#16164,#16165,#16166,#16167,#16168,#16169,#16170,
#16171,#16172,#16173),.UNSPECIFIED.,.F.,.F.,(4,3,3,3,3,3,3,3,3,3,3,3,3,
3,3,3,3,4),(0.,0.0745637565188147,0.124999999999995,0.166238958053025,0.208865678848304,
0.249999999999991,0.346113958897021,0.44432471974493,0.499999999999994,
0.562499999999995,0.623864871544663,0.68693243577233,0.744023847861239,
0.749999999999997,0.824321378787994,0.897946690630251,0.96837154638694,
1.),.UNSPECIFIED.);
#267=B_SPLINE_CURVE_WITH_KNOTS('',3,(#16175,#16176,#16177,#16178),
 .UNSPECIFIED.,.F.,.F.,(4,4),(0.,1.),.UNSPECIFIED.);
#268=B_SPLINE_CURVE_WITH_KNOTS('',3,(#16183,#16184,#16185,#16186,#16187,
#16188,#16189,#16190,#16191,#16192,#16193,#16194,#16195,#16196,#16197,#16198,
#16199,#16200,#16201,#16202,#16203,#16204,#16205,#16206,#16207,#16208,#16209,
#16210,#16211,#16212,#16213,#16214,#16215,#16216,#16217,#16218,#16219,#16220,
#16221,#16222,#16223,#16224,#16225,#16226,#16227,#16228,#16229,#16230,#16231,
#16232,#16233,#16234,#16235,#16236),.UNSPECIFIED.,.F.,.F.,(4,2,2,2,1,1,
2,2,2,2,2,2,2,2,2,2,1,1,2,2,2,2,2,2,2,2,2,2,4),(0.,0.0625000000000705,0.0937500000001039,
0.109375000000121,0.117187500000129,0.121093750000133,0.123046875000136,
0.125000000000139,0.187500000000148,0.218750000000152,0.250000000000156,
0.312500000000164,0.343750000000167,0.37500000000017,0.437500000000176,
0.468750000000182,0.484375000000184,0.492187500000182,0.496093750000183,
0.500000000000184,0.625000000000146,0.687500000000124,0.718750000000111,
0.734375000000106,0.7500000000001,0.812500000000071,0.84375000000006,0.875000000000048,
1.),.UNSPECIFIED.);
#269=B_SPLINE_CURVE_WITH_KNOTS('',3,(#16244,#16245,#16246,#16247,#16248,
#16249,#16250,#16251,#16252,#16253,#16254,#16255,#16256,#16257,#16258,#16259,
#16260,#16261,#16262,#16263,#16264,#16265,#16266,#16267,#16268,#16269,#16270,
#16271,#16272,#16273,#16274,#16275,#16276,#16277,#16278,#16279,#16280,#16281,
#16282,#16283,#16284,#16285,#16286,#16287,#16288,#16289,#16290,#16291,#16292,
#16293,#16294,#16295),.UNSPECIFIED.,.F.,.F.,(4,3,3,3,3,3,3,3,3,3,3,3,3,
3,3,3,3,4),(0.,0.0745637565509513,0.125,0.166238958062739,0.208865678867621,
0.25,0.346113958735942,0.444324719419348,0.5,0.5625,0.623864871537258,0.686932435768629,
0.74402384785074,0.75,0.824321356610985,0.897946645963302,0.968371480101265,
0.999999995426981),.UNSPECIFIED.);
#270=B_SPLINE_CURVE_WITH_KNOTS('',3,(#16770,#16771,#16772,#16773),
 .UNSPECIFIED.,.F.,.F.,(4,4),(0.,1.),.UNSPECIFIED.);
#271=B_SPLINE_CURVE_WITH_KNOTS('',3,(#16782,#16783,#16784,#16785),
 .UNSPECIFIED.,.F.,.F.,(4,4),(0.,1.),.UNSPECIFIED.);
#272=B_SPLINE_CURVE_WITH_KNOTS('',3,(#16789,#16790,#16791,#16792),
 .UNSPECIFIED.,.F.,.F.,(4,4),(0.,1.),.UNSPECIFIED.);
#273=B_SPLINE_CURVE_WITH_KNOTS('',3,(#16802,#16803,#16804,#16805),
 .UNSPECIFIED.,.F.,.F.,(4,4),(0.,1.),.UNSPECIFIED.);
#274=B_SPLINE_CURVE_WITH_KNOTS('',3,(#16814,#16815,#16816,#16817),
 .UNSPECIFIED.,.F.,.F.,(4,4),(0.,1.),.UNSPECIFIED.);
#275=B_SPLINE_CURVE_WITH_KNOTS('',3,(#16826,#16827,#16828,#16829),
 .UNSPECIFIED.,.F.,.F.,(4,4),(0.,1.),.UNSPECIFIED.);
#276=B_SPLINE_CURVE_WITH_KNOTS('',3,(#16833,#16834,#16835,#16836),
 .UNSPECIFIED.,.F.,.F.,(4,4),(0.,1.),.UNSPECIFIED.);
#277=B_SPLINE_CURVE_WITH_KNOTS('',3,(#16846,#16847,#16848,#16849),
 .UNSPECIFIED.,.F.,.F.,(4,4),(0.,1.),.UNSPECIFIED.);
#278=B_SPLINE_CURVE_WITH_KNOTS('',3,(#16858,#16859,#16860,#16861),
 .UNSPECIFIED.,.F.,.F.,(4,4),(0.,1.),.UNSPECIFIED.);
#279=B_SPLINE_CURVE_WITH_KNOTS('',3,(#16870,#16871,#16872,#16873),
 .UNSPECIFIED.,.F.,.F.,(4,4),(0.,1.),.UNSPECIFIED.);
#280=B_SPLINE_CURVE_WITH_KNOTS('',3,(#16877,#16878,#16879,#16880),
 .UNSPECIFIED.,.F.,.F.,(4,4),(0.,1.),.UNSPECIFIED.);
#281=B_SPLINE_CURVE_WITH_KNOTS('',3,(#16890,#16891,#16892,#16893),
 .UNSPECIFIED.,.F.,.F.,(4,4),(0.,1.),.UNSPECIFIED.);
#282=B_SPLINE_CURVE_WITH_KNOTS('',3,(#17701,#17702,#17703,#17704,#17705,
#17706,#17707,#17708,#17709,#17710,#17711,#17712,#17713,#17714,#17715,#17716,
#17717,#17718,#17719,#17720,#17721,#17722,#17723,#17724,#17725,#17726,#17727,
#17728,#17729,#17730,#17731,#17732,#17733,#17734,#17735,#17736,#17737,#17738,
#17739,#17740,#17741,#17742,#17743,#17744,#17745,#17746,#17747,#17748,#17749,
#17750,#17751,#17752,#17753,#17754),.UNSPECIFIED.,.F.,.F.,(4,2,2,2,1,1,
2,2,2,2,2,2,2,2,2,2,1,1,2,2,2,2,2,2,2,2,2,2,4),(0.,0.0624999999999807,0.093749999999971,
0.109374999999966,0.117187499999965,0.121093749999965,0.123046874999964,
0.124999999999963,0.187499999999964,0.218749999999966,0.249999999999968,
0.312499999999973,0.343749999999976,0.37499999999998,0.437499999999987,
0.468749999999992,0.484374999999994,0.492187499999996,0.496093749999996,
0.499999999999996,0.625000000000009,0.687500000000016,0.718750000000018,
0.734375000000018,0.750000000000018,0.812500000000013,0.843750000000011,
0.875000000000008,1.),.UNSPECIFIED.);
#283=B_SPLINE_CURVE_WITH_KNOTS('',3,(#17756,#17757,#17758,#17759,#17760,
#17761,#17762,#17763,#17764,#17765,#17766,#17767,#17768,#17769,#17770,#17771,
#17772,#17773,#17774,#17775,#17776,#17777,#17778,#17779,#17780,#17781,#17782,
#17783,#17784,#17785,#17786,#17787,#17788,#17789,#17790,#17791,#17792,#17793,
#17794,#17795,#17796,#17797,#17798,#17799,#17800,#17801,#17802,#17803,#17804,
#17805,#17806,#17807,#17808,#17809,#17810,#17811,#17812,#17813,#17814,#17815,
#17816,#17817,#17818,#17819,#17820,#17821,#17822,#17823,#17824,#17825,#17826,
#17827,#17828,#17829,#17830,#17831,#17832,#17833,#17834,#17835,#17836,#17837,
#17838,#17839,#17840,#17841,#17842,#17843,#17844,#17845,#17846,#17847,#17848,
#17849,#17850,#17851,#17852,#17853,#17854,#17855,#17856,#17857,#17858,#17859,
#17860,#17861,#17862,#17863,#17864,#17865,#17866,#17867,#17868,#17869,#17870,
#17871,#17872,#17873,#17874,#17875,#17876,#17877,#17878,#17879,#17880,#17881,
#17882,#17883,#17884,#17885,#17886,#17887,#17888,#17889,#17890,#17891,#17892,
#17893,#17894,#17895,#17896,#17897,#17898,#17899,#17900,#17901,#17902,#17903,
#17904,#17905,#17906,#17907,#17908,#17909,#17910,#17911,#17912,#17913,#17914,
#17915,#17916,#17917,#17918,#17919,#17920,#17921,#17922,#17923,#17924,#17925,
#17926,#17927,#17928,#17929,#17930,#17931,#17932,#17933,#17934,#17935,#17936),
 .UNSPECIFIED.,.F.,.F.,(4,3,3,3,3,3,3,3,3,3,3,3,3,3,3,3,3,3,3,3,3,3,3,3,
3,3,3,3,3,3,3,3,3,3,3,3,3,3,3,3,3,3,3,3,3,3,3,3,3,3,3,3,3,3,3,3,3,3,3,3,
4),(0.,0.0533325059154056,0.062500000000017,0.0841085084223245,0.105548099835893,
0.125000000000034,0.17630092547998,0.187500000000051,0.21875000000006,0.234375000000064,
0.242187500000064,0.2475481526123,0.250000000000065,0.287437188884715,0.323763744367256,
0.360010308275466,0.393976204354617,0.427224027414522,0.45953710653336,
0.468750000000096,0.484375000000098,0.492187500000099,0.496093750000102,
0.499047272544739,0.500000000000104,0.531406909072734,0.56257845453641,
0.593750000000087,0.605659576246251,0.617496842260655,0.625000000000081,
0.661169076083868,0.687500000000069,0.718750000000065,0.734375000000062,
0.742187500000061,0.750000000000059,0.781516758434333,0.812500000000044,
0.832471682711535,0.852007989016106,0.870840276699918,0.875000000000029,
0.897518269572018,0.906250000000022,0.921875000000018,0.929687500000018,
0.934543491257381,0.937500000000019,0.950765546817596,0.963898373867096,
0.968750000000011,0.978633754201887,0.984375000000007,0.991614644761784,
0.992187500000004,0.994140625000003,0.995507742863477,0.996093750000002,
0.998075415535184,1.),.UNSPECIFIED.);
#284=B_SPLINE_CURVE_WITH_KNOTS('',3,(#17938,#17939,#17940,#17941,#17942,
#17943,#17944,#17945,#17946,#17947,#17948,#17949,#17950,#17951,#17952,#17953,
#17954,#17955,#17956,#17957,#17958,#17959,#17960,#17961,#17962,#17963,#17964,
#17965,#17966,#17967,#17968,#17969,#17970,#17971,#17972,#17973,#17974,#17975,
#17976,#17977,#17978,#17979,#17980,#17981,#17982,#17983,#17984,#17985,#17986,
#17987,#17988,#17989,#17990,#17991,#17992,#17993,#17994,#17995,#17996,#17997,
#17998,#17999,#18000,#18001,#18002,#18003,#18004,#18005,#18006,#18007,#18008,
#18009,#18010,#18011,#18012,#18013,#18014,#18015,#18016,#18017,#18018,#18019,
#18020,#18021,#18022,#18023,#18024,#18025,#18026,#18027,#18028,#18029,#18030,
#18031,#18032,#18033,#18034,#18035,#18036,#18037,#18038,#18039,#18040,#18041,
#18042,#18043,#18044,#18045,#18046,#18047,#18048,#18049,#18050,#18051,#18052,
#18053,#18054,#18055,#18056,#18057,#18058,#18059,#18060,#18061,#18062,#18063,
#18064,#18065,#18066,#18067,#18068,#18069,#18070,#18071,#18072,#18073,#18074,
#18075,#18076,#18077,#18078,#18079,#18080,#18081,#18082,#18083,#18084,#18085,
#18086,#18087,#18088,#18089,#18090,#18091,#18092,#18093,#18094,#18095,#18096,
#18097,#18098,#18099,#18100,#18101,#18102,#18103,#18104,#18105,#18106,#18107,
#18108,#18109,#18110,#18111,#18112,#18113,#18114,#18115,#18116,#18117,#18118),
 .UNSPECIFIED.,.F.,.F.,(4,3,3,3,3,3,3,3,3,3,3,3,3,3,3,3,3,3,3,3,3,3,3,3,
3,3,3,3,3,3,3,3,3,3,3,3,3,3,3,3,3,3,3,3,3,3,3,3,3,3,3,3,3,3,3,3,3,3,3,3,
4),(0.,0.053332505916002,0.0625000000000664,0.0841085085020462,0.105548099995911,
0.125000000000133,0.176300925460898,0.187500000000199,0.218750000000231,
0.234375000000248,0.242187500000256,0.247548152608829,0.250000000000264,
0.287437188887554,0.323763744372456,0.360010308279463,0.393976204361919,
0.427224027424111,0.459537106542875,0.468750000000484,0.484375000000498,
0.492187500000504,0.496093750000504,0.499047272547063,0.500000000000505,
0.531250000000472,0.562500000000438,0.593750000000407,0.605659576239387,
0.617496842248128,0.625000000000376,0.661011309028678,0.697853969089471,
0.718750000000282,0.734375000000266,0.742187500000258,0.750000000000251,
0.781516758445273,0.812500000000191,0.832471681935561,0.85200798749801,
0.870840274446439,0.875000000000132,0.897518269314931,0.906250000000102,
0.921875000000087,0.92968750000008,0.934543491553856,0.937500000000074,
0.950765490114461,0.963898262934216,0.96875000000004,0.978633529008707,
0.984375000000022,0.991614027021566,0.992187500000011,0.994140625000009,
0.995507744224286,0.996093750000006,0.998075415565434,1.),.UNSPECIFIED.);
#285=B_SPLINE_CURVE_WITH_KNOTS('',3,(#18120,#18121,#18122,#18123,#18124,
#18125,#18126,#18127,#18128,#18129,#18130,#18131,#18132,#18133,#18134,#18135,
#18136,#18137,#18138,#18139,#18140,#18141,#18142,#18143,#18144,#18145,#18146,
#18147,#18148,#18149,#18150,#18151,#18152,#18153,#18154,#18155,#18156,#18157,
#18158,#18159,#18160,#18161,#18162,#18163,#18164,#18165,#18166,#18167,#18168,
#18169,#18170,#18171,#18172,#18173),.UNSPECIFIED.,.F.,.F.,(4,2,2,2,1,1,
2,2,2,2,2,2,2,2,2,2,1,1,2,2,2,2,2,2,2,2,2,2,4),(0.,0.0625000000000238,0.0937500000000341,
0.109375000000038,0.11718750000004,0.12109375000004,0.123046875000041,0.125000000000041,
0.187500000000023,0.218750000000015,0.250000000000006,0.312499999999989,
0.343749999999983,0.374999999999977,0.437499999999965,0.468749999999959,
0.484374999999956,0.492187499999955,0.496093749999954,0.499999999999953,
0.624999999999966,0.687499999999976,0.71874999999998,0.734374999999982,
0.749999999999985,0.812499999999992,0.843749999999994,0.874999999999997,
1.),.UNSPECIFIED.);
#286=B_SPLINE_CURVE_WITH_KNOTS('',3,(#18175,#18176,#18177,#18178,#18179,
#18180,#18181,#18182,#18183,#18184,#18185,#18186,#18187,#18188,#18189,#18190,
#18191,#18192,#18193,#18194,#18195,#18196,#18197,#18198,#18199,#18200,#18201,
#18202,#18203,#18204,#18205,#18206,#18207,#18208,#18209,#18210,#18211,#18212,
#18213,#18214,#18215,#18216,#18217,#18218,#18219,#18220,#18221,#18222,#18223,
#18224,#18225,#18226,#18227,#18228),.UNSPECIFIED.,.F.,.F.,(4,2,2,2,1,1,
2,2,2,2,2,2,2,2,2,2,1,1,2,2,2,2,2,2,2,2,2,2,4),(0.,0.0625000000000846,0.093750000000127,
0.109375000000148,0.117187500000158,0.121093750000162,0.123046875000163,
0.125000000000164,0.187500000000187,0.2187500000002,0.250000000000213,0.312500000000245,
0.343750000000259,0.375000000000273,0.437500000000297,0.468750000000308,
0.484375000000314,0.492187500000316,0.496093750000316,0.500000000000315,
0.625000000000258,0.687500000000227,0.718750000000211,0.734375000000202,
0.750000000000193,0.812500000000147,0.843750000000123,0.875000000000099,
1.),.UNSPECIFIED.);
#287=B_SPLINE_CURVE_WITH_KNOTS('',3,(#18230,#18231,#18232,#18233,#18234,
#18235,#18236,#18237,#18238,#18239,#18240,#18241,#18242,#18243,#18244,#18245,
#18246,#18247,#18248,#18249,#18250,#18251,#18252,#18253,#18254,#18255,#18256,
#18257,#18258,#18259,#18260,#18261,#18262,#18263,#18264,#18265,#18266,#18267,
#18268,#18269,#18270,#18271,#18272,#18273,#18274,#18275,#18276,#18277,#18278,
#18279,#18280,#18281,#18282,#18283,#18284,#18285,#18286,#18287,#18288,#18289,
#18290,#18291,#18292,#18293,#18294,#18295,#18296,#18297,#18298,#18299,#18300,
#18301,#18302,#18303,#18304,#18305,#18306,#18307,#18308,#18309,#18310,#18311,
#18312,#18313,#18314,#18315,#18316,#18317,#18318,#18319,#18320,#18321,#18322,
#18323,#18324,#18325,#18326,#18327,#18328,#18329,#18330,#18331,#18332,#18333,
#18334,#18335,#18336,#18337,#18338,#18339,#18340,#18341,#18342,#18343,#18344,
#18345,#18346,#18347,#18348,#18349,#18350,#18351,#18352,#18353,#18354,#18355,
#18356,#18357,#18358,#18359,#18360,#18361,#18362,#18363,#18364,#18365,#18366,
#18367,#18368,#18369,#18370,#18371,#18372,#18373,#18374,#18375,#18376,#18377,
#18378,#18379,#18380,#18381,#18382,#18383,#18384,#18385,#18386,#18387,#18388,
#18389,#18390,#18391,#18392,#18393,#18394,#18395,#18396,#18397,#18398,#18399,
#18400,#18401,#18402,#18403,#18404,#18405,#18406,#18407,#18408,#18409,#18410),
 .UNSPECIFIED.,.F.,.F.,(4,3,3,3,3,3,3,3,3,3,3,3,3,3,3,3,3,3,3,3,3,3,3,3,
3,3,3,3,3,3,3,3,3,3,3,3,3,3,3,3,3,3,3,3,3,3,3,3,3,3,3,3,3,3,3,3,3,3,3,3,
4),(0.,0.05335209394236,0.062500000000007,0.0841472767069337,0.105624836390271,
0.125000000000014,0.176300925463353,0.187500000000021,0.218750000000026,
0.234375000000029,0.24218750000003,0.247548152609244,0.250000000000031,
0.287437188886521,0.323763744370703,0.360010308278026,0.393976204358943,
0.427224027420569,0.459537106532236,0.468749999999997,0.484374999999994,
0.492187499999994,0.496093749999994,0.499047272546512,0.499999999999994,
0.531406909114999,0.562578454557502,0.593750000000005,0.605659576241387,
0.617496842252372,0.625000000000008,0.661011309019872,0.69785396907197,
0.718750000000017,0.734375000000017,0.742187500000017,0.750000000000017,
0.781516758358948,0.812500000000015,0.83247168165504,0.852007986946234,
0.870840273623334,0.875000000000014,0.897518269153575,0.906250000000012,
0.921875000000012,0.929687500000011,0.934543491364392,0.937500000000009,
0.950765509160406,0.963898300247594,0.968750000000007,0.978633643598403,
0.984375000000004,0.991614445716802,0.992187500000004,0.994140625000004,
0.995507743246036,0.996093750000003,0.998075415497727,1.),.UNSPECIFIED.);
#288=B_SPLINE_CURVE_WITH_KNOTS('',3,(#19003,#19004,#19005,#19006,#19007,
#19008,#19009,#19010,#19011,#19012,#19013,#19014,#19015,#19016),
 .UNSPECIFIED.,.F.,.F.,(4,2,2,2,2,2,4),(1.0000000090833E-6,0.0397704331538061,
0.0783295476556165,0.10311510516028,0.130769699028325,0.170261252779255,
0.207364811990595),.UNSPECIFIED.);
#289=B_SPLINE_CURVE_WITH_KNOTS('',3,(#19045,#19046,#19047,#19048,#19049,
#19050,#19051,#19052,#19053,#19054,#19055,#19056,#19057,#19058),
 .UNSPECIFIED.,.F.,.F.,(4,2,2,2,2,2,4),(1.00000005137352E-6,0.0364150080452644,
0.0751701681205766,0.102306577132939,0.126714048144896,0.164687443503408,
0.20385265381537),.UNSPECIFIED.);
#290=B_SPLINE_CURVE_WITH_KNOTS('',3,(#19129,#19130,#19131,#19132,#19133,
#19134,#19135,#19136,#19137,#19138,#19139,#19140,#19141,#19142),
 .UNSPECIFIED.,.F.,.F.,(4,2,2,2,2,2,4),(1.00000002985316E-6,0.0497274416726429,
0.101777541549185,0.213706159601663,0.317575823833734,0.371841554247195,
0.427578702498277),.UNSPECIFIED.);
#291=B_SPLINE_CURVE_WITH_KNOTS('',3,(#19182,#19183,#19184,#19185,#19186,
#19187,#19188,#19189,#19190,#19191,#19192,#19193,#19194,#19195),
 .UNSPECIFIED.,.F.,.F.,(4,2,2,2,2,2,4),(1.00000005253209E-6,0.0558510119021626,
0.110229405327848,0.214323647321834,0.326650579970185,0.379079827251892,
0.429160855957136),.UNSPECIFIED.);
#292=(
BOUNDED_SURFACE()
B_SPLINE_SURFACE(2,2,((#15889,#15890,#15891),(#15892,#15893,#15894),(#15895,
#15896,#15897),(#15898,#15899,#15900),(#15901,#15902,#15903)),
 .UNSPECIFIED.,.F.,.F.,.F.)
B_SPLINE_SURFACE_WITH_KNOTS((3,2,3),(3,3),(-1.57079650760589,-0.785398253794349,
1.7193274521714E-11),(-6.45261621924302E-12,1.57079632720499),
 .UNSPECIFIED.)
GEOMETRIC_REPRESENTATION_ITEM()
RATIONAL_B_SPLINE_SURFACE(((1.,0.707106781039276,1.),(0.923879515211315,
0.6532814700692,0.923879515211315),(1.,0.707106781039276,1.),(0.923879515211332,
0.653281470069212,0.923879515211332),(1.,0.707106781039276,1.)))
REPRESENTATION_ITEM('')
SURFACE()
);
#293=(
BOUNDED_SURFACE()
B_SPLINE_SURFACE(2,2,((#15907,#15908,#15909),(#15910,#15911,#15912),(#15913,
#15914,#15915),(#15916,#15917,#15918),(#15919,#15920,#15921)),
 .UNSPECIFIED.,.F.,.F.,.F.)
B_SPLINE_SURFACE_WITH_KNOTS((3,2,3),(3,3),(-1.21879451958182E-11,0.785398208598734,
1.57079641720966),(-1.18060512023842E-11,1.57079632732992),
 .UNSPECIFIED.)
GEOMETRIC_REPRESENTATION_ITEM()
RATIONAL_B_SPLINE_SURFACE(((1.,0.707106780993216,1.),(0.923879523860082,
0.653281476142247,0.923879523860082),(1.,0.707106780993216,1.),(0.923879523860064,
0.653281476142235,0.923879523860064),(1.,0.707106780993216,1.)))
REPRESENTATION_ITEM('')
SURFACE()
);
#294=SHAPE_REPRESENTATION_RELATIONSHIP('SRR','None',#20256,#306);
#295=SHAPE_REPRESENTATION_RELATIONSHIP('SRR','None',#20257,#307);
#296=SHAPE_REPRESENTATION_RELATIONSHIP('SRR','None',#20258,#308);
#297=SHAPE_REPRESENTATION_RELATIONSHIP('SRR','None',#20259,#309);
#298=SHAPE_REPRESENTATION_RELATIONSHIP('SRR','None',#20261,#310);
#299=SHAPE_REPRESENTATION_RELATIONSHIP('SRR','None',#20262,#311);
#300=SHAPE_REPRESENTATION_RELATIONSHIP('SRR','None',#20264,#312);
#301=SHAPE_REPRESENTATION_RELATIONSHIP('SRR','None',#20265,#313);
#302=SHAPE_REPRESENTATION_RELATIONSHIP('SRR','None',#20266,#314);
#303=SHAPE_REPRESENTATION_RELATIONSHIP('SRR','None',#20267,#315);
#304=SHAPE_REPRESENTATION_RELATIONSHIP('SRR','None',#20268,#316);
#305=SHAPE_REPRESENTATION_RELATIONSHIP('SRR','None',#20269,#317);
#306=ADVANCED_BREP_SHAPE_REPRESENTATION('',(#353),#20162);
#307=ADVANCED_BREP_SHAPE_REPRESENTATION('',(#354),#20163);
#308=ADVANCED_BREP_SHAPE_REPRESENTATION('',(#355),#20164);
#309=ADVANCED_BREP_SHAPE_REPRESENTATION('',(#356),#20165);
#310=ADVANCED_BREP_SHAPE_REPRESENTATION('',(#357),#20167);
#311=ADVANCED_BREP_SHAPE_REPRESENTATION('',(#358),#20168);
#312=ADVANCED_BREP_SHAPE_REPRESENTATION('',(#359),#20170);
#313=ADVANCED_BREP_SHAPE_REPRESENTATION('',(#360,#361,#362,#363,#364,#365,
#366,#367,#368,#369,#370,#371,#372,#373,#374,#375),#20171);
#314=ADVANCED_BREP_SHAPE_REPRESENTATION('',(#376),#20172);
#315=ADVANCED_BREP_SHAPE_REPRESENTATION('',(#377),#20173);
#316=ADVANCED_BREP_SHAPE_REPRESENTATION('',(#378),#20174);
#317=ADVANCED_BREP_SHAPE_REPRESENTATION('',(#379),#20175);
#318=STYLED_ITEM('',(#20335),#353);
#319=STYLED_ITEM('',(#20336),#354);
#320=STYLED_ITEM('',(#20334),#355);
#321=STYLED_ITEM('',(#20334),#195);
#322=STYLED_ITEM('',(#20334),#196);
#323=STYLED_ITEM('',(#20334),#197);
#324=STYLED_ITEM('',(#20334),#198);
#325=STYLED_ITEM('',(#20334),#199);
#326=STYLED_ITEM('',(#20334),#200);
#327=STYLED_ITEM('',(#20334),#201);
#328=STYLED_ITEM('',(#20334),#202);
#329=STYLED_ITEM('',(#20337),#356);
#330=STYLED_ITEM('',(#20337),#357);
#331=STYLED_ITEM('',(#20337),#358);
#332=STYLED_ITEM('',(#20338),#359);
#333=STYLED_ITEM('',(#20338),#360);
#334=STYLED_ITEM('',(#20338),#361);
#335=STYLED_ITEM('',(#20338),#362);
#336=STYLED_ITEM('',(#20338),#363);
#337=STYLED_ITEM('',(#20338),#364);
#338=STYLED_ITEM('',(#20338),#365);
#339=STYLED_ITEM('',(#20338),#366);
#340=STYLED_ITEM('',(#20338),#367);
#341=STYLED_ITEM('',(#20338),#368);
#342=STYLED_ITEM('',(#20338),#369);
#343=STYLED_ITEM('',(#20338),#370);
#344=STYLED_ITEM('',(#20338),#371);
#345=STYLED_ITEM('',(#20338),#372);
#346=STYLED_ITEM('',(#20338),#373);
#347=STYLED_ITEM('',(#20338),#374);
#348=STYLED_ITEM('',(#20338),#375);
#349=STYLED_ITEM('',(#20337),#376);
#350=STYLED_ITEM('',(#20337),#377);
#351=STYLED_ITEM('',(#20337),#378);
#352=STYLED_ITEM('',(#20337),#379);
#353=MANIFOLD_SOLID_BREP('Body1',#10944);
#354=MANIFOLD_SOLID_BREP('Body1',#10945);
#355=MANIFOLD_SOLID_BREP('Body1',#10946);
#356=MANIFOLD_SOLID_BREP('Body1',#10947);
#357=MANIFOLD_SOLID_BREP('Body1',#10948);
#358=MANIFOLD_SOLID_BREP('Body1',#10949);
#359=MANIFOLD_SOLID_BREP('Body1',#10950);
#360=MANIFOLD_SOLID_BREP('Body1',#10951);
#361=MANIFOLD_SOLID_BREP('Body2',#10952);
#362=MANIFOLD_SOLID_BREP('Body3',#10953);
#363=MANIFOLD_SOLID_BREP('Body4',#10954);
#364=MANIFOLD_SOLID_BREP('Body5',#10955);
#365=MANIFOLD_SOLID_BREP('Body6',#10956);
#366=MANIFOLD_SOLID_BREP('Body7',#10957);
#367=MANIFOLD_SOLID_BREP('Body8',#10958);
#368=MANIFOLD_SOLID_BREP('Body9',#10959);
#369=MANIFOLD_SOLID_BREP('Body10',#10960);
#370=MANIFOLD_SOLID_BREP('Body11',#10961);
#371=MANIFOLD_SOLID_BREP('Body12',#10962);
#372=MANIFOLD_SOLID_BREP('Body13',#10963);
#373=MANIFOLD_SOLID_BREP('Body14',#10964);
#374=MANIFOLD_SOLID_BREP('Body15',#10965);
#375=MANIFOLD_SOLID_BREP('Body16',#10966);
#376=MANIFOLD_SOLID_BREP('Body1',#10967);
#377=MANIFOLD_SOLID_BREP('Body1',#10968);
#378=MANIFOLD_SOLID_BREP('Body1',#10969);
#379=MANIFOLD_SOLID_BREP('Body1',#10970);
#380=FACE_BOUND('',#1518,.T.);
#381=FACE_BOUND('',#1519,.T.);
#382=FACE_BOUND('',#1520,.T.);
#383=FACE_BOUND('',#1521,.T.);
#384=FACE_BOUND('',#1524,.T.);
#385=FACE_BOUND('',#1525,.T.);
#386=FACE_BOUND('',#1526,.T.);
#387=FACE_BOUND('',#1527,.T.);
#388=FACE_BOUND('',#1530,.T.);
#389=FACE_BOUND('',#1531,.T.);
#390=FACE_BOUND('',#1532,.T.);
#391=FACE_BOUND('',#1533,.T.);
#392=FACE_BOUND('',#1534,.T.);
#393=FACE_BOUND('',#1535,.T.);
#394=FACE_BOUND('',#1536,.T.);
#395=FACE_BOUND('',#1537,.T.);
#396=FACE_BOUND('',#1538,.T.);
#397=FACE_BOUND('',#1541,.T.);
#398=FACE_BOUND('',#1542,.T.);
#399=FACE_BOUND('',#1543,.T.);
#400=FACE_BOUND('',#1544,.T.);
#401=FACE_BOUND('',#1547,.T.);
#402=FACE_BOUND('',#1548,.T.);
#403=FACE_BOUND('',#1549,.T.);
#404=FACE_BOUND('',#1550,.T.);
#405=FACE_BOUND('',#1553,.T.);
#406=FACE_BOUND('',#1554,.T.);
#407=FACE_BOUND('',#1555,.T.);
#408=FACE_BOUND('',#1556,.T.);
#409=FACE_BOUND('',#1557,.T.);
#410=FACE_BOUND('',#1558,.T.);
#411=FACE_BOUND('',#1559,.T.);
#412=FACE_BOUND('',#1560,.T.);
#413=FACE_BOUND('',#1561,.T.);
#414=FACE_BOUND('',#1600,.T.);
#415=FACE_BOUND('',#1606,.T.);
#416=FACE_BOUND('',#1619,.T.);
#417=FACE_BOUND('',#1620,.T.);
#418=FACE_BOUND('',#1621,.T.);
#419=FACE_BOUND('',#1622,.T.);
#420=FACE_BOUND('',#1623,.T.);
#421=FACE_BOUND('',#1624,.T.);
#422=FACE_BOUND('',#1632,.T.);
#423=FACE_BOUND('',#1633,.T.);
#424=FACE_BOUND('',#1634,.T.);
#425=FACE_BOUND('',#1635,.T.);
#426=FACE_BOUND('',#1636,.T.);
#427=FACE_BOUND('',#1637,.T.);
#428=FACE_BOUND('',#1643,.T.);
#429=FACE_BOUND('',#1685,.T.);
#430=FACE_BOUND('',#1739,.T.);
#431=FACE_BOUND('',#1741,.T.);
#432=FACE_BOUND('',#1743,.T.);
#433=FACE_BOUND('',#1745,.T.);
#434=FACE_BOUND('',#1747,.T.);
#435=FACE_BOUND('',#1749,.T.);
#436=FACE_BOUND('',#1816,.T.);
#437=FACE_BOUND('',#1818,.T.);
#438=FACE_BOUND('',#1820,.T.);
#439=FACE_BOUND('',#1822,.T.);
#440=FACE_BOUND('',#1824,.T.);
#441=FACE_BOUND('',#1826,.T.);
#442=FACE_BOUND('',#1839,.T.);
#443=FACE_BOUND('',#1848,.T.);
#444=FACE_BOUND('',#1875,.T.);
#445=FACE_BOUND('',#1881,.T.);
#446=FACE_BOUND('',#1910,.T.);
#447=FACE_BOUND('',#1913,.T.);
#448=FACE_BOUND('',#1915,.T.);
#449=FACE_BOUND('',#1917,.T.);
#450=FACE_BOUND('',#1962,.T.);
#451=FACE_BOUND('',#1963,.T.);
#452=FACE_BOUND('',#1964,.T.);
#453=FACE_BOUND('',#1965,.T.);
#454=FACE_BOUND('',#1966,.T.);
#455=FACE_BOUND('',#1967,.T.);
#456=FACE_BOUND('',#1968,.T.);
#457=FACE_BOUND('',#1969,.T.);
#458=FACE_BOUND('',#1970,.T.);
#459=FACE_BOUND('',#1971,.T.);
#460=FACE_BOUND('',#1972,.T.);
#461=FACE_BOUND('',#1973,.T.);
#462=FACE_BOUND('',#1974,.T.);
#463=FACE_BOUND('',#1975,.T.);
#464=FACE_BOUND('',#1976,.T.);
#465=FACE_BOUND('',#1977,.T.);
#466=FACE_BOUND('',#1978,.T.);
#467=FACE_BOUND('',#1979,.T.);
#468=FACE_BOUND('',#1980,.T.);
#469=FACE_BOUND('',#1981,.T.);
#470=FACE_BOUND('',#1982,.T.);
#471=FACE_BOUND('',#1983,.T.);
#472=FACE_BOUND('',#1984,.T.);
#473=FACE_BOUND('',#1985,.T.);
#474=FACE_BOUND('',#1986,.T.);
#475=FACE_BOUND('',#1994,.T.);
#476=FACE_BOUND('',#1995,.T.);
#477=FACE_BOUND('',#1996,.T.);
#478=FACE_BOUND('',#1997,.T.);
#479=FACE_BOUND('',#1998,.T.);
#480=FACE_BOUND('',#1999,.T.);
#481=FACE_BOUND('',#2000,.T.);
#482=FACE_BOUND('',#2001,.T.);
#483=FACE_BOUND('',#2002,.T.);
#484=FACE_BOUND('',#2003,.T.);
#485=FACE_BOUND('',#2004,.T.);
#486=FACE_BOUND('',#2005,.T.);
#487=FACE_BOUND('',#2006,.T.);
#488=FACE_BOUND('',#2007,.T.);
#489=FACE_BOUND('',#2008,.T.);
#490=FACE_BOUND('',#2009,.T.);
#491=FACE_BOUND('',#2010,.T.);
#492=FACE_BOUND('',#2011,.T.);
#493=FACE_BOUND('',#2012,.T.);
#494=FACE_BOUND('',#2013,.T.);
#495=FACE_BOUND('',#2014,.T.);
#496=FACE_BOUND('',#2015,.T.);
#497=FACE_BOUND('',#2016,.T.);
#498=FACE_BOUND('',#2017,.T.);
#499=FACE_BOUND('',#2018,.T.);
#500=FACE_BOUND('',#2020,.T.);
#501=FACE_BOUND('',#2021,.T.);
#502=FACE_BOUND('',#2022,.T.);
#503=FACE_BOUND('',#2023,.T.);
#504=FACE_BOUND('',#2027,.T.);
#505=FACE_BOUND('',#2028,.T.);
#506=FACE_BOUND('',#2029,.T.);
#507=FACE_BOUND('',#2030,.T.);
#508=FACE_BOUND('',#2046,.T.);
#509=FACE_BOUND('',#2047,.T.);
#510=FACE_BOUND('',#2048,.T.);
#511=FACE_BOUND('',#2049,.T.);
#512=FACE_BOUND('',#2051,.T.);
#513=FACE_BOUND('',#2052,.T.);
#514=FACE_BOUND('',#2053,.T.);
#515=FACE_BOUND('',#2054,.T.);
#516=FACE_BOUND('',#2077,.T.);
#517=FACE_BOUND('',#2078,.T.);
#518=FACE_BOUND('',#2079,.T.);
#519=FACE_BOUND('',#2080,.T.);
#520=FACE_BOUND('',#2081,.T.);
#521=FACE_BOUND('',#2082,.T.);
#522=FACE_BOUND('',#2083,.T.);
#523=FACE_BOUND('',#2084,.T.);
#524=FACE_BOUND('',#2085,.T.);
#525=FACE_BOUND('',#2086,.T.);
#526=FACE_BOUND('',#2088,.T.);
#527=FACE_BOUND('',#2089,.T.);
#528=FACE_BOUND('',#2090,.T.);
#529=FACE_BOUND('',#2091,.T.);
#530=FACE_BOUND('',#2092,.T.);
#531=FACE_BOUND('',#2093,.T.);
#532=FACE_BOUND('',#2094,.T.);
#533=FACE_BOUND('',#2095,.T.);
#534=FACE_BOUND('',#2096,.T.);
#535=FACE_BOUND('',#2097,.T.);
#536=FACE_BOUND('',#2109,.T.);
#537=FACE_BOUND('',#2110,.T.);
#538=FACE_BOUND('',#2111,.T.);
#539=FACE_BOUND('',#2117,.T.);
#540=FACE_BOUND('',#2118,.T.);
#541=FACE_BOUND('',#2119,.T.);
#542=FACE_BOUND('',#2125,.T.);
#543=FACE_BOUND('',#2126,.T.);
#544=FACE_BOUND('',#2128,.T.);
#545=FACE_BOUND('',#2129,.T.);
#546=FACE_BOUND('',#2149,.T.);
#547=FACE_BOUND('',#2150,.T.);
#548=FACE_BOUND('',#2153,.T.);
#549=FACE_BOUND('',#2154,.T.);
#550=FACE_BOUND('',#2157,.T.);
#551=FACE_BOUND('',#2158,.T.);
#552=FACE_BOUND('',#2160,.T.);
#553=FACE_BOUND('',#2161,.T.);
#554=FACE_BOUND('',#2174,.T.);
#555=FACE_BOUND('',#2177,.T.);
#556=FACE_BOUND('',#2188,.T.);
#557=FACE_BOUND('',#2190,.T.);
#558=FACE_BOUND('',#2206,.T.);
#559=FACE_BOUND('',#2208,.T.);
#560=FACE_BOUND('',#2212,.T.);
#561=FACE_BOUND('',#2214,.T.);
#562=FACE_BOUND('',#2222,.T.);
#563=FACE_BOUND('',#2224,.T.);
#564=FACE_BOUND('',#2226,.T.);
#565=FACE_BOUND('',#2231,.T.);
#566=FACE_BOUND('',#2233,.T.);
#567=FACE_BOUND('',#2235,.T.);
#568=FACE_BOUND('',#2240,.T.);
#569=FACE_BOUND('',#2242,.T.);
#570=FACE_BOUND('',#2244,.T.);
#571=FACE_BOUND('',#2251,.T.);
#572=FACE_BOUND('',#2252,.T.);
#573=FACE_BOUND('',#2254,.T.);
#574=FACE_BOUND('',#2255,.T.);
#575=FACE_BOUND('',#2266,.T.);
#576=PLANE('',#11157);
#577=PLANE('',#11160);
#578=PLANE('',#11161);
#579=PLANE('',#11164);
#580=PLANE('',#11165);
#581=PLANE('',#11168);
#582=PLANE('',#11169);
#583=PLANE('',#11172);
#584=PLANE('',#11173);
#585=PLANE('',#11178);
#586=PLANE('',#11179);
#587=PLANE('',#11185);
#588=PLANE('',#11187);
#589=PLANE('',#11192);
#590=PLANE('',#11193);
#591=PLANE('',#11199);
#592=PLANE('',#11201);
#593=PLANE('',#11202);
#594=PLANE('',#11203);
#595=PLANE('',#11204);
#596=PLANE('',#11205);
#597=PLANE('',#11206);
#598=PLANE('',#11282);
#599=PLANE('',#11295);
#600=PLANE('',#11296);
#601=PLANE('',#11301);
#602=PLANE('',#11303);
#603=PLANE('',#11305);
#604=PLANE('',#11315);
#605=PLANE('',#11350);
#606=PLANE('',#11363);
#607=PLANE('',#11364);
#608=PLANE('',#11365);
#609=PLANE('',#11366);
#610=PLANE('',#11367);
#611=PLANE('',#11368);
#612=PLANE('',#11371);
#613=PLANE('',#11374);
#614=PLANE('',#11379);
#615=PLANE('',#11384);
#616=PLANE('',#11387);
#617=PLANE('',#11393);
#618=PLANE('',#11396);
#619=PLANE('',#11399);
#620=PLANE('',#11402);
#621=PLANE('',#11405);
#622=PLANE('',#11408);
#623=PLANE('',#11411);
#624=PLANE('',#11414);
#625=PLANE('',#11417);
#626=PLANE('',#11420);
#627=PLANE('',#11423);
#628=PLANE('',#11427);
#629=PLANE('',#11428);
#630=PLANE('',#11433);
#631=PLANE('',#11434);
#632=PLANE('',#11435);
#633=PLANE('',#11436);
#634=PLANE('',#11437);
#635=PLANE('',#11440);
#636=PLANE('',#11445);
#637=PLANE('',#11450);
#638=PLANE('',#11453);
#639=PLANE('',#11458);
#640=PLANE('',#11459);
#641=PLANE('',#11460);
#642=PLANE('',#11461);
#643=PLANE('',#11462);
#644=PLANE('',#11466);
#645=PLANE('',#11467);
#646=PLANE('',#11468);
#647=PLANE('',#11469);
#648=PLANE('',#11470);
#649=PLANE('',#11471);
#650=PLANE('',#11472);
#651=PLANE('',#11473);
#652=PLANE('',#11474);
#653=PLANE('',#11475);
#654=PLANE('',#11476);
#655=PLANE('',#11477);
#656=PLANE('',#11478);
#657=PLANE('',#11479);
#658=PLANE('',#11480);
#659=PLANE('',#11481);
#660=PLANE('',#11482);
#661=PLANE('',#11483);
#662=PLANE('',#11484);
#663=PLANE('',#11485);
#664=PLANE('',#11486);
#665=PLANE('',#11487);
#666=PLANE('',#11488);
#667=PLANE('',#11489);
#668=PLANE('',#11490);
#669=PLANE('',#11491);
#670=PLANE('',#11492);
#671=PLANE('',#11493);
#672=PLANE('',#11494);
#673=PLANE('',#11495);
#674=PLANE('',#11496);
#675=PLANE('',#11497);
#676=PLANE('',#11498);
#677=PLANE('',#11499);
#678=PLANE('',#11500);
#679=PLANE('',#11501);
#680=PLANE('',#11502);
#681=PLANE('',#11503);
#682=PLANE('',#11504);
#683=PLANE('',#11505);
#684=PLANE('',#11506);
#685=PLANE('',#11507);
#686=PLANE('',#11508);
#687=PLANE('',#11509);
#688=PLANE('',#11510);
#689=PLANE('',#11511);
#690=PLANE('',#11512);
#691=PLANE('',#11513);
#692=PLANE('',#11514);
#693=PLANE('',#11515);
#694=PLANE('',#11516);
#695=PLANE('',#11517);
#696=PLANE('',#11518);
#697=PLANE('',#11519);
#698=PLANE('',#11520);
#699=PLANE('',#11556);
#700=PLANE('',#11557);
#701=PLANE('',#11558);
#702=PLANE('',#11559);
#703=PLANE('',#11560);
#704=PLANE('',#11561);
#705=PLANE('',#11562);
#706=PLANE('',#11563);
#707=PLANE('',#11564);
#708=PLANE('',#11565);
#709=PLANE('',#11566);
#710=PLANE('',#11567);
#711=PLANE('',#11568);
#712=PLANE('',#11569);
#713=PLANE('',#11570);
#714=PLANE('',#11571);
#715=PLANE('',#11572);
#716=PLANE('',#11573);
#717=PLANE('',#11574);
#718=PLANE('',#11575);
#719=PLANE('',#11576);
#720=PLANE('',#11577);
#721=PLANE('',#11578);
#722=PLANE('',#11579);
#723=PLANE('',#11580);
#724=PLANE('',#11581);
#725=PLANE('',#11582);
#726=PLANE('',#11586);
#727=PLANE('',#11587);
#728=PLANE('',#11588);
#729=PLANE('',#11589);
#730=PLANE('',#11590);
#731=PLANE('',#11591);
#732=PLANE('',#11592);
#733=PLANE('',#11593);
#734=PLANE('',#11594);
#735=PLANE('',#11595);
#736=PLANE('',#11596);
#737=PLANE('',#11597);
#738=PLANE('',#11598);
#739=PLANE('',#11599);
#740=PLANE('',#11600);
#741=PLANE('',#11601);
#742=PLANE('',#11602);
#743=PLANE('',#11603);
#744=PLANE('',#11604);
#745=PLANE('',#11605);
#746=PLANE('',#11606);
#747=PLANE('',#11607);
#748=PLANE('',#11608);
#749=PLANE('',#11609);
#750=PLANE('',#11610);
#751=PLANE('',#11611);
#752=PLANE('',#11612);
#753=PLANE('',#11613);
#754=PLANE('',#11614);
#755=PLANE('',#11615);
#756=PLANE('',#11616);
#757=PLANE('',#11617);
#758=PLANE('',#11618);
#759=PLANE('',#11619);
#760=PLANE('',#11620);
#761=PLANE('',#11621);
#762=PLANE('',#11622);
#763=PLANE('',#11623);
#764=PLANE('',#11624);
#765=PLANE('',#11625);
#766=PLANE('',#11626);
#767=PLANE('',#11627);
#768=PLANE('',#11628);
#769=PLANE('',#11629);
#770=PLANE('',#11630);
#771=PLANE('',#11631);
#772=PLANE('',#11632);
#773=PLANE('',#11633);
#774=PLANE('',#11634);
#775=PLANE('',#11641);
#776=PLANE('',#11642);
#777=PLANE('',#11643);
#778=PLANE('',#11644);
#779=PLANE('',#11645);
#780=PLANE('',#11646);
#781=PLANE('',#11647);
#782=PLANE('',#11648);
#783=PLANE('',#11649);
#784=PLANE('',#11650);
#785=PLANE('',#11651);
#786=PLANE('',#11652);
#787=PLANE('',#11653);
#788=PLANE('',#11654);
#789=PLANE('',#11655);
#790=PLANE('',#11656);
#791=PLANE('',#11657);
#792=PLANE('',#11658);
#793=PLANE('',#11659);
#794=PLANE('',#11660);
#795=PLANE('',#11661);
#796=PLANE('',#11662);
#797=PLANE('',#11663);
#798=PLANE('',#11664);
#799=PLANE('',#11665);
#800=PLANE('',#11666);
#801=PLANE('',#11667);
#802=PLANE('',#11668);
#803=PLANE('',#11669);
#804=PLANE('',#11670);
#805=PLANE('',#11671);
#806=PLANE('',#11672);
#807=PLANE('',#11673);
#808=PLANE('',#11792);
#809=PLANE('',#11798);
#810=PLANE('',#11806);
#811=PLANE('',#11809);
#812=PLANE('',#11810);
#813=PLANE('',#11814);
#814=PLANE('',#11822);
#815=PLANE('',#11827);
#816=PLANE('',#11830);
#817=PLANE('',#11835);
#818=PLANE('',#11838);
#819=PLANE('',#11839);
#820=PLANE('',#11840);
#821=PLANE('',#11841);
#822=PLANE('',#11900);
#823=PLANE('',#11903);
#824=PLANE('',#11908);
#825=PLANE('',#11909);
#826=PLANE('',#11930);
#827=PLANE('',#11931);
#828=PLANE('',#11932);
#829=PLANE('',#11933);
#830=PLANE('',#11934);
#831=PLANE('',#11935);
#832=PLANE('',#11936);
#833=PLANE('',#11940);
#834=PLANE('',#11941);
#835=PLANE('',#11942);
#836=PLANE('',#11946);
#837=PLANE('',#11951);
#838=PLANE('',#11952);
#839=PLANE('',#11953);
#840=PLANE('',#11957);
#841=PLANE('',#11958);
#842=PLANE('',#11959);
#843=PLANE('',#11960);
#844=PLANE('',#11961);
#845=PLANE('',#11962);
#846=PLANE('',#11980);
#847=PLANE('',#11981);
#848=PLANE('',#11982);
#849=PLANE('',#11983);
#850=PLANE('',#11984);
#851=PLANE('',#11985);
#852=PLANE('',#11986);
#853=PLANE('',#11987);
#854=PLANE('',#11988);
#855=PLANE('',#11989);
#856=PLANE('',#11990);
#857=PLANE('',#11991);
#858=PLANE('',#11992);
#859=PLANE('',#11996);
#860=PLANE('',#11997);
#861=PLANE('',#12004);
#862=PLANE('',#12005);
#863=PLANE('',#12006);
#864=PLANE('',#12007);
#865=PLANE('',#12008);
#866=PLANE('',#12009);
#867=PLANE('',#12027);
#868=PLANE('',#12028);
#869=PLANE('',#12059);
#870=PLANE('',#12060);
#871=PLANE('',#12067);
#872=PLANE('',#12068);
#873=PLANE('',#12086);
#874=PLANE('',#12087);
#875=PLANE('',#12088);
#876=PLANE('',#12099);
#877=PLANE('',#12100);
#878=PLANE('',#12101);
#879=PLANE('',#12112);
#880=PLANE('',#12113);
#881=PLANE('',#12114);
#882=PLANE('',#12144);
#883=PLANE('',#12146);
#884=PLANE('',#12149);
#885=PLANE('',#12150);
#886=PLANE('',#12171);
#887=PLANE('',#12172);
#888=PLANE('',#12173);
#889=PLANE('',#12174);
#890=PLANE('',#12175);
#891=PLANE('',#12176);
#892=PLANE('',#12177);
#893=PLANE('',#12178);
#894=PLANE('',#12179);
#895=PLANE('',#12180);
#896=PLANE('',#12181);
#897=PLANE('',#12182);
#898=PLANE('',#12183);
#899=PLANE('',#12184);
#900=FACE_OUTER_BOUND('',#1492,.T.);
#901=FACE_OUTER_BOUND('',#1493,.T.);
#902=FACE_OUTER_BOUND('',#1494,.T.);
#903=FACE_OUTER_BOUND('',#1495,.T.);
#904=FACE_OUTER_BOUND('',#1496,.T.);
#905=FACE_OUTER_BOUND('',#1497,.T.);
#906=FACE_OUTER_BOUND('',#1498,.T.);
#907=FACE_OUTER_BOUND('',#1499,.T.);
#908=FACE_OUTER_BOUND('',#1500,.T.);
#909=FACE_OUTER_BOUND('',#1501,.T.);
#910=FACE_OUTER_BOUND('',#1502,.T.);
#911=FACE_OUTER_BOUND('',#1503,.T.);
#912=FACE_OUTER_BOUND('',#1504,.T.);
#913=FACE_OUTER_BOUND('',#1505,.T.);
#914=FACE_OUTER_BOUND('',#1506,.T.);
#915=FACE_OUTER_BOUND('',#1507,.T.);
#916=FACE_OUTER_BOUND('',#1508,.T.);
#917=FACE_OUTER_BOUND('',#1509,.T.);
#918=FACE_OUTER_BOUND('',#1510,.T.);
#919=FACE_OUTER_BOUND('',#1511,.T.);
#920=FACE_OUTER_BOUND('',#1512,.T.);
#921=FACE_OUTER_BOUND('',#1513,.T.);
#922=FACE_OUTER_BOUND('',#1514,.T.);
#923=FACE_OUTER_BOUND('',#1515,.T.);
#924=FACE_OUTER_BOUND('',#1516,.T.);
#925=FACE_OUTER_BOUND('',#1517,.T.);
#926=FACE_OUTER_BOUND('',#1522,.T.);
#927=FACE_OUTER_BOUND('',#1523,.T.);
#928=FACE_OUTER_BOUND('',#1528,.T.);
#929=FACE_OUTER_BOUND('',#1529,.T.);
#930=FACE_OUTER_BOUND('',#1539,.T.);
#931=FACE_OUTER_BOUND('',#1540,.T.);
#932=FACE_OUTER_BOUND('',#1545,.T.);
#933=FACE_OUTER_BOUND('',#1546,.T.);
#934=FACE_OUTER_BOUND('',#1551,.T.);
#935=FACE_OUTER_BOUND('',#1552,.T.);
#936=FACE_OUTER_BOUND('',#1562,.T.);
#937=FACE_OUTER_BOUND('',#1563,.T.);
#938=FACE_OUTER_BOUND('',#1564,.T.);
#939=FACE_OUTER_BOUND('',#1565,.T.);
#940=FACE_OUTER_BOUND('',#1566,.T.);
#941=FACE_OUTER_BOUND('',#1567,.T.);
#942=FACE_OUTER_BOUND('',#1568,.T.);
#943=FACE_OUTER_BOUND('',#1569,.T.);
#944=FACE_OUTER_BOUND('',#1570,.T.);
#945=FACE_OUTER_BOUND('',#1571,.T.);
#946=FACE_OUTER_BOUND('',#1572,.T.);
#947=FACE_OUTER_BOUND('',#1573,.T.);
#948=FACE_OUTER_BOUND('',#1574,.T.);
#949=FACE_OUTER_BOUND('',#1575,.T.);
#950=FACE_OUTER_BOUND('',#1576,.T.);
#951=FACE_OUTER_BOUND('',#1577,.T.);
#952=FACE_OUTER_BOUND('',#1578,.T.);
#953=FACE_OUTER_BOUND('',#1579,.T.);
#954=FACE_OUTER_BOUND('',#1580,.T.);
#955=FACE_OUTER_BOUND('',#1581,.T.);
#956=FACE_OUTER_BOUND('',#1582,.T.);
#957=FACE_OUTER_BOUND('',#1583,.T.);
#958=FACE_OUTER_BOUND('',#1584,.T.);
#959=FACE_OUTER_BOUND('',#1585,.T.);
#960=FACE_OUTER_BOUND('',#1586,.T.);
#961=FACE_OUTER_BOUND('',#1587,.T.);
#962=FACE_OUTER_BOUND('',#1588,.T.);
#963=FACE_OUTER_BOUND('',#1589,.T.);
#964=FACE_OUTER_BOUND('',#1590,.T.);
#965=FACE_OUTER_BOUND('',#1591,.T.);
#966=FACE_OUTER_BOUND('',#1592,.T.);
#967=FACE_OUTER_BOUND('',#1593,.T.);
#968=FACE_OUTER_BOUND('',#1594,.T.);
#969=FACE_OUTER_BOUND('',#1595,.T.);
#970=FACE_OUTER_BOUND('',#1596,.T.);
#971=FACE_OUTER_BOUND('',#1597,.T.);
#972=FACE_OUTER_BOUND('',#1598,.T.);
#973=FACE_OUTER_BOUND('',#1599,.T.);
#974=FACE_OUTER_BOUND('',#1601,.T.);
#975=FACE_OUTER_BOUND('',#1602,.T.);
#976=FACE_OUTER_BOUND('',#1603,.T.);
#977=FACE_OUTER_BOUND('',#1604,.T.);
#978=FACE_OUTER_BOUND('',#1605,.T.);
#979=FACE_OUTER_BOUND('',#1607,.T.);
#980=FACE_OUTER_BOUND('',#1608,.T.);
#981=FACE_OUTER_BOUND('',#1609,.T.);
#982=FACE_OUTER_BOUND('',#1610,.T.);
#983=FACE_OUTER_BOUND('',#1611,.T.);
#984=FACE_OUTER_BOUND('',#1612,.T.);
#985=FACE_OUTER_BOUND('',#1613,.T.);
#986=FACE_OUTER_BOUND('',#1614,.T.);
#987=FACE_OUTER_BOUND('',#1615,.T.);
#988=FACE_OUTER_BOUND('',#1616,.T.);
#989=FACE_OUTER_BOUND('',#1617,.T.);
#990=FACE_OUTER_BOUND('',#1618,.T.);
#991=FACE_OUTER_BOUND('',#1625,.T.);
#992=FACE_OUTER_BOUND('',#1626,.T.);
#993=FACE_OUTER_BOUND('',#1627,.T.);
#994=FACE_OUTER_BOUND('',#1628,.T.);
#995=FACE_OUTER_BOUND('',#1629,.T.);
#996=FACE_OUTER_BOUND('',#1630,.T.);
#997=FACE_OUTER_BOUND('',#1631,.T.);
#998=FACE_OUTER_BOUND('',#1638,.T.);
#999=FACE_OUTER_BOUND('',#1639,.T.);
#1000=FACE_OUTER_BOUND('',#1640,.T.);
#1001=FACE_OUTER_BOUND('',#1641,.T.);
#1002=FACE_OUTER_BOUND('',#1642,.T.);
#1003=FACE_OUTER_BOUND('',#1644,.T.);
#1004=FACE_OUTER_BOUND('',#1645,.T.);
#1005=FACE_OUTER_BOUND('',#1646,.T.);
#1006=FACE_OUTER_BOUND('',#1647,.T.);
#1007=FACE_OUTER_BOUND('',#1648,.T.);
#1008=FACE_OUTER_BOUND('',#1649,.T.);
#1009=FACE_OUTER_BOUND('',#1650,.T.);
#1010=FACE_OUTER_BOUND('',#1651,.T.);
#1011=FACE_OUTER_BOUND('',#1652,.T.);
#1012=FACE_OUTER_BOUND('',#1653,.T.);
#1013=FACE_OUTER_BOUND('',#1654,.T.);
#1014=FACE_OUTER_BOUND('',#1655,.T.);
#1015=FACE_OUTER_BOUND('',#1656,.T.);
#1016=FACE_OUTER_BOUND('',#1657,.T.);
#1017=FACE_OUTER_BOUND('',#1658,.T.);
#1018=FACE_OUTER_BOUND('',#1659,.T.);
#1019=FACE_OUTER_BOUND('',#1660,.T.);
#1020=FACE_OUTER_BOUND('',#1661,.T.);
#1021=FACE_OUTER_BOUND('',#1662,.T.);
#1022=FACE_OUTER_BOUND('',#1663,.T.);
#1023=FACE_OUTER_BOUND('',#1664,.T.);
#1024=FACE_OUTER_BOUND('',#1665,.T.);
#1025=FACE_OUTER_BOUND('',#1666,.T.);
#1026=FACE_OUTER_BOUND('',#1667,.T.);
#1027=FACE_OUTER_BOUND('',#1668,.T.);
#1028=FACE_OUTER_BOUND('',#1669,.T.);
#1029=FACE_OUTER_BOUND('',#1670,.T.);
#1030=FACE_OUTER_BOUND('',#1671,.T.);
#1031=FACE_OUTER_BOUND('',#1672,.T.);
#1032=FACE_OUTER_BOUND('',#1673,.T.);
#1033=FACE_OUTER_BOUND('',#1674,.T.);
#1034=FACE_OUTER_BOUND('',#1675,.T.);
#1035=FACE_OUTER_BOUND('',#1676,.T.);
#1036=FACE_OUTER_BOUND('',#1677,.T.);
#1037=FACE_OUTER_BOUND('',#1678,.T.);
#1038=FACE_OUTER_BOUND('',#1679,.T.);
#1039=FACE_OUTER_BOUND('',#1680,.T.);
#1040=FACE_OUTER_BOUND('',#1681,.T.);
#1041=FACE_OUTER_BOUND('',#1682,.T.);
#1042=FACE_OUTER_BOUND('',#1683,.T.);
#1043=FACE_OUTER_BOUND('',#1684,.T.);
#1044=FACE_OUTER_BOUND('',#1686,.T.);
#1045=FACE_OUTER_BOUND('',#1687,.T.);
#1046=FACE_OUTER_BOUND('',#1688,.T.);
#1047=FACE_OUTER_BOUND('',#1689,.T.);
#1048=FACE_OUTER_BOUND('',#1690,.T.);
#1049=FACE_OUTER_BOUND('',#1691,.T.);
#1050=FACE_OUTER_BOUND('',#1692,.T.);
#1051=FACE_OUTER_BOUND('',#1693,.T.);
#1052=FACE_OUTER_BOUND('',#1694,.T.);
#1053=FACE_OUTER_BOUND('',#1695,.T.);
#1054=FACE_OUTER_BOUND('',#1696,.T.);
#1055=FACE_OUTER_BOUND('',#1697,.T.);
#1056=FACE_OUTER_BOUND('',#1698,.T.);
#1057=FACE_OUTER_BOUND('',#1699,.T.);
#1058=FACE_OUTER_BOUND('',#1700,.T.);
#1059=FACE_OUTER_BOUND('',#1701,.T.);
#1060=FACE_OUTER_BOUND('',#1702,.T.);
#1061=FACE_OUTER_BOUND('',#1703,.T.);
#1062=FACE_OUTER_BOUND('',#1704,.T.);
#1063=FACE_OUTER_BOUND('',#1705,.T.);
#1064=FACE_OUTER_BOUND('',#1706,.T.);
#1065=FACE_OUTER_BOUND('',#1707,.T.);
#1066=FACE_OUTER_BOUND('',#1708,.T.);
#1067=FACE_OUTER_BOUND('',#1709,.T.);
#1068=FACE_OUTER_BOUND('',#1710,.T.);
#1069=FACE_OUTER_BOUND('',#1711,.T.);
#1070=FACE_OUTER_BOUND('',#1712,.T.);
#1071=FACE_OUTER_BOUND('',#1713,.T.);
#1072=FACE_OUTER_BOUND('',#1714,.T.);
#1073=FACE_OUTER_BOUND('',#1715,.T.);
#1074=FACE_OUTER_BOUND('',#1716,.T.);
#1075=FACE_OUTER_BOUND('',#1717,.T.);
#1076=FACE_OUTER_BOUND('',#1718,.T.);
#1077=FACE_OUTER_BOUND('',#1719,.T.);
#1078=FACE_OUTER_BOUND('',#1720,.T.);
#1079=FACE_OUTER_BOUND('',#1721,.T.);
#1080=FACE_OUTER_BOUND('',#1722,.T.);
#1081=FACE_OUTER_BOUND('',#1723,.T.);
#1082=FACE_OUTER_BOUND('',#1724,.T.);
#1083=FACE_OUTER_BOUND('',#1725,.T.);
#1084=FACE_OUTER_BOUND('',#1726,.T.);
#1085=FACE_OUTER_BOUND('',#1727,.T.);
#1086=FACE_OUTER_BOUND('',#1728,.T.);
#1087=FACE_OUTER_BOUND('',#1729,.T.);
#1088=FACE_OUTER_BOUND('',#1730,.T.);
#1089=FACE_OUTER_BOUND('',#1731,.T.);
#1090=FACE_OUTER_BOUND('',#1732,.T.);
#1091=FACE_OUTER_BOUND('',#1733,.T.);
#1092=FACE_OUTER_BOUND('',#1734,.T.);
#1093=FACE_OUTER_BOUND('',#1735,.T.);
#1094=FACE_OUTER_BOUND('',#1736,.T.);
#1095=FACE_OUTER_BOUND('',#1737,.T.);
#1096=FACE_OUTER_BOUND('',#1738,.T.);
#1097=FACE_OUTER_BOUND('',#1740,.T.);
#1098=FACE_OUTER_BOUND('',#1742,.T.);
#1099=FACE_OUTER_BOUND('',#1744,.T.);
#1100=FACE_OUTER_BOUND('',#1746,.T.);
#1101=FACE_OUTER_BOUND('',#1748,.T.);
#1102=FACE_OUTER_BOUND('',#1750,.T.);
#1103=FACE_OUTER_BOUND('',#1751,.T.);
#1104=FACE_OUTER_BOUND('',#1752,.T.);
#1105=FACE_OUTER_BOUND('',#1753,.T.);
#1106=FACE_OUTER_BOUND('',#1754,.T.);
#1107=FACE_OUTER_BOUND('',#1755,.T.);
#1108=FACE_OUTER_BOUND('',#1756,.T.);
#1109=FACE_OUTER_BOUND('',#1757,.T.);
#1110=FACE_OUTER_BOUND('',#1758,.T.);
#1111=FACE_OUTER_BOUND('',#1759,.T.);
#1112=FACE_OUTER_BOUND('',#1760,.T.);
#1113=FACE_OUTER_BOUND('',#1761,.T.);
#1114=FACE_OUTER_BOUND('',#1762,.T.);
#1115=FACE_OUTER_BOUND('',#1763,.T.);
#1116=FACE_OUTER_BOUND('',#1764,.T.);
#1117=FACE_OUTER_BOUND('',#1765,.T.);
#1118=FACE_OUTER_BOUND('',#1766,.T.);
#1119=FACE_OUTER_BOUND('',#1767,.T.);
#1120=FACE_OUTER_BOUND('',#1768,.T.);
#1121=FACE_OUTER_BOUND('',#1769,.T.);
#1122=FACE_OUTER_BOUND('',#1770,.T.);
#1123=FACE_OUTER_BOUND('',#1771,.T.);
#1124=FACE_OUTER_BOUND('',#1772,.T.);
#1125=FACE_OUTER_BOUND('',#1773,.T.);
#1126=FACE_OUTER_BOUND('',#1774,.T.);
#1127=FACE_OUTER_BOUND('',#1775,.T.);
#1128=FACE_OUTER_BOUND('',#1776,.T.);
#1129=FACE_OUTER_BOUND('',#1777,.T.);
#1130=FACE_OUTER_BOUND('',#1778,.T.);
#1131=FACE_OUTER_BOUND('',#1779,.T.);
#1132=FACE_OUTER_BOUND('',#1780,.T.);
#1133=FACE_OUTER_BOUND('',#1781,.T.);
#1134=FACE_OUTER_BOUND('',#1782,.T.);
#1135=FACE_OUTER_BOUND('',#1783,.T.);
#1136=FACE_OUTER_BOUND('',#1784,.T.);
#1137=FACE_OUTER_BOUND('',#1785,.T.);
#1138=FACE_OUTER_BOUND('',#1786,.T.);
#1139=FACE_OUTER_BOUND('',#1787,.T.);
#1140=FACE_OUTER_BOUND('',#1788,.T.);
#1141=FACE_OUTER_BOUND('',#1789,.T.);
#1142=FACE_OUTER_BOUND('',#1790,.T.);
#1143=FACE_OUTER_BOUND('',#1791,.T.);
#1144=FACE_OUTER_BOUND('',#1792,.T.);
#1145=FACE_OUTER_BOUND('',#1793,.T.);
#1146=FACE_OUTER_BOUND('',#1794,.T.);
#1147=FACE_OUTER_BOUND('',#1795,.T.);
#1148=FACE_OUTER_BOUND('',#1796,.T.);
#1149=FACE_OUTER_BOUND('',#1797,.T.);
#1150=FACE_OUTER_BOUND('',#1798,.T.);
#1151=FACE_OUTER_BOUND('',#1799,.T.);
#1152=FACE_OUTER_BOUND('',#1800,.T.);
#1153=FACE_OUTER_BOUND('',#1801,.T.);
#1154=FACE_OUTER_BOUND('',#1802,.T.);
#1155=FACE_OUTER_BOUND('',#1803,.T.);
#1156=FACE_OUTER_BOUND('',#1804,.T.);
#1157=FACE_OUTER_BOUND('',#1805,.T.);
#1158=FACE_OUTER_BOUND('',#1806,.T.);
#1159=FACE_OUTER_BOUND('',#1807,.T.);
#1160=FACE_OUTER_BOUND('',#1808,.T.);
#1161=FACE_OUTER_BOUND('',#1809,.T.);
#1162=FACE_OUTER_BOUND('',#1810,.T.);
#1163=FACE_OUTER_BOUND('',#1811,.T.);
#1164=FACE_OUTER_BOUND('',#1812,.T.);
#1165=FACE_OUTER_BOUND('',#1813,.T.);
#1166=FACE_OUTER_BOUND('',#1814,.T.);
#1167=FACE_OUTER_BOUND('',#1815,.T.);
#1168=FACE_OUTER_BOUND('',#1817,.T.);
#1169=FACE_OUTER_BOUND('',#1819,.T.);
#1170=FACE_OUTER_BOUND('',#1821,.T.);
#1171=FACE_OUTER_BOUND('',#1823,.T.);
#1172=FACE_OUTER_BOUND('',#1825,.T.);
#1173=FACE_OUTER_BOUND('',#1827,.T.);
#1174=FACE_OUTER_BOUND('',#1828,.T.);
#1175=FACE_OUTER_BOUND('',#1829,.T.);
#1176=FACE_OUTER_BOUND('',#1830,.T.);
#1177=FACE_OUTER_BOUND('',#1831,.T.);
#1178=FACE_OUTER_BOUND('',#1832,.T.);
#1179=FACE_OUTER_BOUND('',#1833,.T.);
#1180=FACE_OUTER_BOUND('',#1834,.T.);
#1181=FACE_OUTER_BOUND('',#1835,.T.);
#1182=FACE_OUTER_BOUND('',#1836,.T.);
#1183=FACE_OUTER_BOUND('',#1837,.T.);
#1184=FACE_OUTER_BOUND('',#1838,.T.);
#1185=FACE_OUTER_BOUND('',#1840,.T.);
#1186=FACE_OUTER_BOUND('',#1841,.T.);
#1187=FACE_OUTER_BOUND('',#1842,.T.);
#1188=FACE_OUTER_BOUND('',#1843,.T.);
#1189=FACE_OUTER_BOUND('',#1844,.T.);
#1190=FACE_OUTER_BOUND('',#1845,.T.);
#1191=FACE_OUTER_BOUND('',#1846,.T.);
#1192=FACE_OUTER_BOUND('',#1847,.T.);
#1193=FACE_OUTER_BOUND('',#1849,.T.);
#1194=FACE_OUTER_BOUND('',#1850,.T.);
#1195=FACE_OUTER_BOUND('',#1851,.T.);
#1196=FACE_OUTER_BOUND('',#1852,.T.);
#1197=FACE_OUTER_BOUND('',#1853,.T.);
#1198=FACE_OUTER_BOUND('',#1854,.T.);
#1199=FACE_OUTER_BOUND('',#1855,.T.);
#1200=FACE_OUTER_BOUND('',#1856,.T.);
#1201=FACE_OUTER_BOUND('',#1857,.T.);
#1202=FACE_OUTER_BOUND('',#1858,.T.);
#1203=FACE_OUTER_BOUND('',#1859,.T.);
#1204=FACE_OUTER_BOUND('',#1860,.T.);
#1205=FACE_OUTER_BOUND('',#1861,.T.);
#1206=FACE_OUTER_BOUND('',#1862,.T.);
#1207=FACE_OUTER_BOUND('',#1863,.T.);
#1208=FACE_OUTER_BOUND('',#1864,.T.);
#1209=FACE_OUTER_BOUND('',#1865,.T.);
#1210=FACE_OUTER_BOUND('',#1866,.T.);
#1211=FACE_OUTER_BOUND('',#1867,.T.);
#1212=FACE_OUTER_BOUND('',#1868,.T.);
#1213=FACE_OUTER_BOUND('',#1869,.T.);
#1214=FACE_OUTER_BOUND('',#1870,.T.);
#1215=FACE_OUTER_BOUND('',#1871,.T.);
#1216=FACE_OUTER_BOUND('',#1872,.T.);
#1217=FACE_OUTER_BOUND('',#1873,.T.);
#1218=FACE_OUTER_BOUND('',#1874,.T.);
#1219=FACE_OUTER_BOUND('',#1876,.T.);
#1220=FACE_OUTER_BOUND('',#1877,.T.);
#1221=FACE_OUTER_BOUND('',#1878,.T.);
#1222=FACE_OUTER_BOUND('',#1879,.T.);
#1223=FACE_OUTER_BOUND('',#1880,.T.);
#1224=FACE_OUTER_BOUND('',#1882,.T.);
#1225=FACE_OUTER_BOUND('',#1883,.T.);
#1226=FACE_OUTER_BOUND('',#1884,.T.);
#1227=FACE_OUTER_BOUND('',#1885,.T.);
#1228=FACE_OUTER_BOUND('',#1886,.T.);
#1229=FACE_OUTER_BOUND('',#1887,.T.);
#1230=FACE_OUTER_BOUND('',#1888,.T.);
#1231=FACE_OUTER_BOUND('',#1889,.T.);
#1232=FACE_OUTER_BOUND('',#1890,.T.);
#1233=FACE_OUTER_BOUND('',#1891,.T.);
#1234=FACE_OUTER_BOUND('',#1892,.T.);
#1235=FACE_OUTER_BOUND('',#1893,.T.);
#1236=FACE_OUTER_BOUND('',#1894,.T.);
#1237=FACE_OUTER_BOUND('',#1895,.T.);
#1238=FACE_OUTER_BOUND('',#1896,.T.);
#1239=FACE_OUTER_BOUND('',#1897,.T.);
#1240=FACE_OUTER_BOUND('',#1898,.T.);
#1241=FACE_OUTER_BOUND('',#1899,.T.);
#1242=FACE_OUTER_BOUND('',#1900,.T.);
#1243=FACE_OUTER_BOUND('',#1901,.T.);
#1244=FACE_OUTER_BOUND('',#1902,.T.);
#1245=FACE_OUTER_BOUND('',#1903,.T.);
#1246=FACE_OUTER_BOUND('',#1904,.T.);
#1247=FACE_OUTER_BOUND('',#1905,.T.);
#1248=FACE_OUTER_BOUND('',#1906,.T.);
#1249=FACE_OUTER_BOUND('',#1907,.T.);
#1250=FACE_OUTER_BOUND('',#1908,.T.);
#1251=FACE_OUTER_BOUND('',#1909,.T.);
#1252=FACE_OUTER_BOUND('',#1911,.T.);
#1253=FACE_OUTER_BOUND('',#1912,.T.);
#1254=FACE_OUTER_BOUND('',#1914,.T.);
#1255=FACE_OUTER_BOUND('',#1916,.T.);
#1256=FACE_OUTER_BOUND('',#1918,.T.);
#1257=FACE_OUTER_BOUND('',#1919,.T.);
#1258=FACE_OUTER_BOUND('',#1920,.T.);
#1259=FACE_OUTER_BOUND('',#1921,.T.);
#1260=FACE_OUTER_BOUND('',#1922,.T.);
#1261=FACE_OUTER_BOUND('',#1923,.T.);
#1262=FACE_OUTER_BOUND('',#1924,.T.);
#1263=FACE_OUTER_BOUND('',#1925,.T.);
#1264=FACE_OUTER_BOUND('',#1926,.T.);
#1265=FACE_OUTER_BOUND('',#1927,.T.);
#1266=FACE_OUTER_BOUND('',#1928,.T.);
#1267=FACE_OUTER_BOUND('',#1929,.T.);
#1268=FACE_OUTER_BOUND('',#1930,.T.);
#1269=FACE_OUTER_BOUND('',#1931,.T.);
#1270=FACE_OUTER_BOUND('',#1932,.T.);
#1271=FACE_OUTER_BOUND('',#1933,.T.);
#1272=FACE_OUTER_BOUND('',#1934,.T.);
#1273=FACE_OUTER_BOUND('',#1935,.T.);
#1274=FACE_OUTER_BOUND('',#1936,.T.);
#1275=FACE_OUTER_BOUND('',#1937,.T.);
#1276=FACE_OUTER_BOUND('',#1938,.T.);
#1277=FACE_OUTER_BOUND('',#1939,.T.);
#1278=FACE_OUTER_BOUND('',#1940,.T.);
#1279=FACE_OUTER_BOUND('',#1941,.T.);
#1280=FACE_OUTER_BOUND('',#1942,.T.);
#1281=FACE_OUTER_BOUND('',#1943,.T.);
#1282=FACE_OUTER_BOUND('',#1944,.T.);
#1283=FACE_OUTER_BOUND('',#1945,.T.);
#1284=FACE_OUTER_BOUND('',#1946,.T.);
#1285=FACE_OUTER_BOUND('',#1947,.T.);
#1286=FACE_OUTER_BOUND('',#1948,.T.);
#1287=FACE_OUTER_BOUND('',#1949,.T.);
#1288=FACE_OUTER_BOUND('',#1950,.T.);
#1289=FACE_OUTER_BOUND('',#1951,.T.);
#1290=FACE_OUTER_BOUND('',#1952,.T.);
#1291=FACE_OUTER_BOUND('',#1953,.T.);
#1292=FACE_OUTER_BOUND('',#1954,.T.);
#1293=FACE_OUTER_BOUND('',#1955,.T.);
#1294=FACE_OUTER_BOUND('',#1956,.T.);
#1295=FACE_OUTER_BOUND('',#1957,.T.);
#1296=FACE_OUTER_BOUND('',#1958,.T.);
#1297=FACE_OUTER_BOUND('',#1959,.T.);
#1298=FACE_OUTER_BOUND('',#1960,.T.);
#1299=FACE_OUTER_BOUND('',#1961,.T.);
#1300=FACE_OUTER_BOUND('',#1987,.T.);
#1301=FACE_OUTER_BOUND('',#1988,.T.);
#1302=FACE_OUTER_BOUND('',#1989,.T.);
#1303=FACE_OUTER_BOUND('',#1990,.T.);
#1304=FACE_OUTER_BOUND('',#1991,.T.);
#1305=FACE_OUTER_BOUND('',#1992,.T.);
#1306=FACE_OUTER_BOUND('',#1993,.T.);
#1307=FACE_OUTER_BOUND('',#2019,.T.);
#1308=FACE_OUTER_BOUND('',#2024,.T.);
#1309=FACE_OUTER_BOUND('',#2025,.T.);
#1310=FACE_OUTER_BOUND('',#2026,.T.);
#1311=FACE_OUTER_BOUND('',#2031,.T.);
#1312=FACE_OUTER_BOUND('',#2032,.T.);
#1313=FACE_OUTER_BOUND('',#2033,.T.);
#1314=FACE_OUTER_BOUND('',#2034,.T.);
#1315=FACE_OUTER_BOUND('',#2035,.T.);
#1316=FACE_OUTER_BOUND('',#2036,.T.);
#1317=FACE_OUTER_BOUND('',#2037,.T.);
#1318=FACE_OUTER_BOUND('',#2038,.T.);
#1319=FACE_OUTER_BOUND('',#2039,.T.);
#1320=FACE_OUTER_BOUND('',#2040,.T.);
#1321=FACE_OUTER_BOUND('',#2041,.T.);
#1322=FACE_OUTER_BOUND('',#2042,.T.);
#1323=FACE_OUTER_BOUND('',#2043,.T.);
#1324=FACE_OUTER_BOUND('',#2044,.T.);
#1325=FACE_OUTER_BOUND('',#2045,.T.);
#1326=FACE_OUTER_BOUND('',#2050,.T.);
#1327=FACE_OUTER_BOUND('',#2055,.T.);
#1328=FACE_OUTER_BOUND('',#2056,.T.);
#1329=FACE_OUTER_BOUND('',#2057,.T.);
#1330=FACE_OUTER_BOUND('',#2058,.T.);
#1331=FACE_OUTER_BOUND('',#2059,.T.);
#1332=FACE_OUTER_BOUND('',#2060,.T.);
#1333=FACE_OUTER_BOUND('',#2061,.T.);
#1334=FACE_OUTER_BOUND('',#2062,.T.);
#1335=FACE_OUTER_BOUND('',#2063,.T.);
#1336=FACE_OUTER_BOUND('',#2064,.T.);
#1337=FACE_OUTER_BOUND('',#2065,.T.);
#1338=FACE_OUTER_BOUND('',#2066,.T.);
#1339=FACE_OUTER_BOUND('',#2067,.T.);
#1340=FACE_OUTER_BOUND('',#2068,.T.);
#1341=FACE_OUTER_BOUND('',#2069,.T.);
#1342=FACE_OUTER_BOUND('',#2070,.T.);
#1343=FACE_OUTER_BOUND('',#2071,.T.);
#1344=FACE_OUTER_BOUND('',#2072,.T.);
#1345=FACE_OUTER_BOUND('',#2073,.T.);
#1346=FACE_OUTER_BOUND('',#2074,.T.);
#1347=FACE_OUTER_BOUND('',#2075,.T.);
#1348=FACE_OUTER_BOUND('',#2076,.T.);
#1349=FACE_OUTER_BOUND('',#2087,.T.);
#1350=FACE_OUTER_BOUND('',#2098,.T.);
#1351=FACE_OUTER_BOUND('',#2099,.T.);
#1352=FACE_OUTER_BOUND('',#2100,.T.);
#1353=FACE_OUTER_BOUND('',#2101,.T.);
#1354=FACE_OUTER_BOUND('',#2102,.T.);
#1355=FACE_OUTER_BOUND('',#2103,.T.);
#1356=FACE_OUTER_BOUND('',#2104,.T.);
#1357=FACE_OUTER_BOUND('',#2105,.T.);
#1358=FACE_OUTER_BOUND('',#2106,.T.);
#1359=FACE_OUTER_BOUND('',#2107,.T.);
#1360=FACE_OUTER_BOUND('',#2108,.T.);
#1361=FACE_OUTER_BOUND('',#2112,.T.);
#1362=FACE_OUTER_BOUND('',#2113,.T.);
#1363=FACE_OUTER_BOUND('',#2114,.T.);
#1364=FACE_OUTER_BOUND('',#2115,.T.);
#1365=FACE_OUTER_BOUND('',#2116,.T.);
#1366=FACE_OUTER_BOUND('',#2120,.T.);
#1367=FACE_OUTER_BOUND('',#2121,.T.);
#1368=FACE_OUTER_BOUND('',#2122,.T.);
#1369=FACE_OUTER_BOUND('',#2123,.T.);
#1370=FACE_OUTER_BOUND('',#2124,.T.);
#1371=FACE_OUTER_BOUND('',#2127,.T.);
#1372=FACE_OUTER_BOUND('',#2130,.T.);
#1373=FACE_OUTER_BOUND('',#2131,.T.);
#1374=FACE_OUTER_BOUND('',#2132,.T.);
#1375=FACE_OUTER_BOUND('',#2133,.T.);
#1376=FACE_OUTER_BOUND('',#2134,.T.);
#1377=FACE_OUTER_BOUND('',#2135,.T.);
#1378=FACE_OUTER_BOUND('',#2136,.T.);
#1379=FACE_OUTER_BOUND('',#2137,.T.);
#1380=FACE_OUTER_BOUND('',#2138,.T.);
#1381=FACE_OUTER_BOUND('',#2139,.T.);
#1382=FACE_OUTER_BOUND('',#2140,.T.);
#1383=FACE_OUTER_BOUND('',#2141,.T.);
#1384=FACE_OUTER_BOUND('',#2142,.T.);
#1385=FACE_OUTER_BOUND('',#2143,.T.);
#1386=FACE_OUTER_BOUND('',#2144,.T.);
#1387=FACE_OUTER_BOUND('',#2145,.T.);
#1388=FACE_OUTER_BOUND('',#2146,.T.);
#1389=FACE_OUTER_BOUND('',#2147,.T.);
#1390=FACE_OUTER_BOUND('',#2148,.T.);
#1391=FACE_OUTER_BOUND('',#2151,.T.);
#1392=FACE_OUTER_BOUND('',#2152,.T.);
#1393=FACE_OUTER_BOUND('',#2155,.T.);
#1394=FACE_OUTER_BOUND('',#2156,.T.);
#1395=FACE_OUTER_BOUND('',#2159,.T.);
#1396=FACE_OUTER_BOUND('',#2162,.T.);
#1397=FACE_OUTER_BOUND('',#2163,.T.);
#1398=FACE_OUTER_BOUND('',#2164,.T.);
#1399=FACE_OUTER_BOUND('',#2165,.T.);
#1400=FACE_OUTER_BOUND('',#2166,.T.);
#1401=FACE_OUTER_BOUND('',#2167,.T.);
#1402=FACE_OUTER_BOUND('',#2168,.T.);
#1403=FACE_OUTER_BOUND('',#2169,.T.);
#1404=FACE_OUTER_BOUND('',#2170,.T.);
#1405=FACE_OUTER_BOUND('',#2171,.T.);
#1406=FACE_OUTER_BOUND('',#2172,.T.);
#1407=FACE_OUTER_BOUND('',#2173,.T.);
#1408=FACE_OUTER_BOUND('',#2175,.T.);
#1409=FACE_OUTER_BOUND('',#2176,.T.);
#1410=FACE_OUTER_BOUND('',#2178,.T.);
#1411=FACE_OUTER_BOUND('',#2179,.T.);
#1412=FACE_OUTER_BOUND('',#2180,.T.);
#1413=FACE_OUTER_BOUND('',#2181,.T.);
#1414=FACE_OUTER_BOUND('',#2182,.T.);
#1415=FACE_OUTER_BOUND('',#2183,.T.);
#1416=FACE_OUTER_BOUND('',#2184,.T.);
#1417=FACE_OUTER_BOUND('',#2185,.T.);
#1418=FACE_OUTER_BOUND('',#2186,.T.);
#1419=FACE_OUTER_BOUND('',#2187,.T.);
#1420=FACE_OUTER_BOUND('',#2189,.T.);
#1421=FACE_OUTER_BOUND('',#2191,.T.);
#1422=FACE_OUTER_BOUND('',#2192,.T.);
#1423=FACE_OUTER_BOUND('',#2193,.T.);
#1424=FACE_OUTER_BOUND('',#2194,.T.);
#1425=FACE_OUTER_BOUND('',#2195,.T.);
#1426=FACE_OUTER_BOUND('',#2196,.T.);
#1427=FACE_OUTER_BOUND('',#2197,.T.);
#1428=FACE_OUTER_BOUND('',#2198,.T.);
#1429=FACE_OUTER_BOUND('',#2199,.T.);
#1430=FACE_OUTER_BOUND('',#2200,.T.);
#1431=FACE_OUTER_BOUND('',#2201,.T.);
#1432=FACE_OUTER_BOUND('',#2202,.T.);
#1433=FACE_OUTER_BOUND('',#2203,.T.);
#1434=FACE_OUTER_BOUND('',#2204,.T.);
#1435=FACE_OUTER_BOUND('',#2205,.T.);
#1436=FACE_OUTER_BOUND('',#2207,.T.);
#1437=FACE_OUTER_BOUND('',#2209,.T.);
#1438=FACE_OUTER_BOUND('',#2210,.T.);
#1439=FACE_OUTER_BOUND('',#2211,.T.);
#1440=FACE_OUTER_BOUND('',#2213,.T.);
#1441=FACE_OUTER_BOUND('',#2215,.T.);
#1442=FACE_OUTER_BOUND('',#2216,.T.);
#1443=FACE_OUTER_BOUND('',#2217,.T.);
#1444=FACE_OUTER_BOUND('',#2218,.T.);
#1445=FACE_OUTER_BOUND('',#2219,.T.);
#1446=FACE_OUTER_BOUND('',#2220,.T.);
#1447=FACE_OUTER_BOUND('',#2221,.T.);
#1448=FACE_OUTER_BOUND('',#2223,.T.);
#1449=FACE_OUTER_BOUND('',#2225,.T.);
#1450=FACE_OUTER_BOUND('',#2227,.T.);
#1451=FACE_OUTER_BOUND('',#2228,.T.);
#1452=FACE_OUTER_BOUND('',#2229,.T.);
#1453=FACE_OUTER_BOUND('',#2230,.T.);
#1454=FACE_OUTER_BOUND('',#2232,.T.);
#1455=FACE_OUTER_BOUND('',#2234,.T.);
#1456=FACE_OUTER_BOUND('',#2236,.T.);
#1457=FACE_OUTER_BOUND('',#2237,.T.);
#1458=FACE_OUTER_BOUND('',#2238,.T.);
#1459=FACE_OUTER_BOUND('',#2239,.T.);
#1460=FACE_OUTER_BOUND('',#2241,.T.);
#1461=FACE_OUTER_BOUND('',#2243,.T.);
#1462=FACE_OUTER_BOUND('',#2245,.T.);
#1463=FACE_OUTER_BOUND('',#2246,.T.);
#1464=FACE_OUTER_BOUND('',#2247,.T.);
#1465=FACE_OUTER_BOUND('',#2248,.T.);
#1466=FACE_OUTER_BOUND('',#2249,.T.);
#1467=FACE_OUTER_BOUND('',#2250,.T.);
#1468=FACE_OUTER_BOUND('',#2253,.T.);
#1469=FACE_OUTER_BOUND('',#2256,.T.);
#1470=FACE_OUTER_BOUND('',#2257,.T.);
#1471=FACE_OUTER_BOUND('',#2258,.T.);
#1472=FACE_OUTER_BOUND('',#2259,.T.);
#1473=FACE_OUTER_BOUND('',#2260,.T.);
#1474=FACE_OUTER_BOUND('',#2261,.T.);
#1475=FACE_OUTER_BOUND('',#2262,.T.);
#1476=FACE_OUTER_BOUND('',#2263,.T.);
#1477=FACE_OUTER_BOUND('',#2264,.T.);
#1478=FACE_OUTER_BOUND('',#2265,.T.);
#1479=FACE_OUTER_BOUND('',#2267,.T.);
#1480=FACE_OUTER_BOUND('',#2268,.T.);
#1481=FACE_OUTER_BOUND('',#2269,.T.);
#1482=FACE_OUTER_BOUND('',#2270,.T.);
#1483=FACE_OUTER_BOUND('',#2271,.T.);
#1484=FACE_OUTER_BOUND('',#2272,.T.);
#1485=FACE_OUTER_BOUND('',#2273,.T.);
#1486=FACE_OUTER_BOUND('',#2274,.T.);
#1487=FACE_OUTER_BOUND('',#2275,.T.);
#1488=FACE_OUTER_BOUND('',#2276,.T.);
#1489=FACE_OUTER_BOUND('',#2277,.T.);
#1490=FACE_OUTER_BOUND('',#2278,.T.);
#1491=FACE_OUTER_BOUND('',#2279,.T.);
#1492=EDGE_LOOP('',(#7183,#7184,#7185,#7186));
#1493=EDGE_LOOP('',(#7187,#7188,#7189,#7190));
#1494=EDGE_LOOP('',(#7191,#7192,#7193,#7194));
#1495=EDGE_LOOP('',(#7195,#7196,#7197,#7198));
#1496=EDGE_LOOP('',(#7199,#7200,#7201,#7202));
#1497=EDGE_LOOP('',(#7203,#7204,#7205,#7206));
#1498=EDGE_LOOP('',(#7207,#7208,#7209,#7210));
#1499=EDGE_LOOP('',(#7211,#7212,#7213,#7214));
#1500=EDGE_LOOP('',(#7215,#7216,#7217,#7218));
#1501=EDGE_LOOP('',(#7219,#7220,#7221,#7222));
#1502=EDGE_LOOP('',(#7223,#7224,#7225,#7226));
#1503=EDGE_LOOP('',(#7227,#7228,#7229,#7230));
#1504=EDGE_LOOP('',(#7231,#7232,#7233,#7234));
#1505=EDGE_LOOP('',(#7235,#7236,#7237,#7238));
#1506=EDGE_LOOP('',(#7239,#7240,#7241,#7242));
#1507=EDGE_LOOP('',(#7243,#7244,#7245,#7246));
#1508=EDGE_LOOP('',(#7247,#7248,#7249,#7250));
#1509=EDGE_LOOP('',(#7251,#7252,#7253,#7254));
#1510=EDGE_LOOP('',(#7255,#7256,#7257,#7258));
#1511=EDGE_LOOP('',(#7259,#7260,#7261,#7262));
#1512=EDGE_LOOP('',(#7263,#7264,#7265,#7266));
#1513=EDGE_LOOP('',(#7267,#7268,#7269,#7270));
#1514=EDGE_LOOP('',(#7271,#7272,#7273,#7274));
#1515=EDGE_LOOP('',(#7275,#7276,#7277,#7278));
#1516=EDGE_LOOP('',(#7279,#7280,#7281,#7282));
#1517=EDGE_LOOP('',(#7283,#7284,#7285,#7286,#7287,#7288,#7289,#7290,#7291,
#7292));
#1518=EDGE_LOOP('',(#7293));
#1519=EDGE_LOOP('',(#7294));
#1520=EDGE_LOOP('',(#7295));
#1521=EDGE_LOOP('',(#7296));
#1522=EDGE_LOOP('',(#7297,#7298,#7299,#7300));
#1523=EDGE_LOOP('',(#7301,#7302,#7303,#7304,#7305,#7306,#7307,#7308,#7309,
#7310));
#1524=EDGE_LOOP('',(#7311));
#1525=EDGE_LOOP('',(#7312));
#1526=EDGE_LOOP('',(#7313));
#1527=EDGE_LOOP('',(#7314));
#1528=EDGE_LOOP('',(#7315,#7316,#7317,#7318));
#1529=EDGE_LOOP('',(#7319,#7320,#7321,#7322));
#1530=EDGE_LOOP('',(#7323));
#1531=EDGE_LOOP('',(#7324));
#1532=EDGE_LOOP('',(#7325));
#1533=EDGE_LOOP('',(#7326));
#1534=EDGE_LOOP('',(#7327));
#1535=EDGE_LOOP('',(#7328));
#1536=EDGE_LOOP('',(#7329));
#1537=EDGE_LOOP('',(#7330));
#1538=EDGE_LOOP('',(#7331));
#1539=EDGE_LOOP('',(#7332,#7333,#7334,#7335));
#1540=EDGE_LOOP('',(#7336,#7337,#7338,#7339,#7340,#7341,#7342,#7343,#7344,
#7345));
#1541=EDGE_LOOP('',(#7346));
#1542=EDGE_LOOP('',(#7347));
#1543=EDGE_LOOP('',(#7348));
#1544=EDGE_LOOP('',(#7349));
#1545=EDGE_LOOP('',(#7350,#7351,#7352,#7353));
#1546=EDGE_LOOP('',(#7354,#7355,#7356,#7357,#7358,#7359,#7360,#7361,#7362,
#7363));
#1547=EDGE_LOOP('',(#7364));
#1548=EDGE_LOOP('',(#7365));
#1549=EDGE_LOOP('',(#7366));
#1550=EDGE_LOOP('',(#7367));
#1551=EDGE_LOOP('',(#7368,#7369,#7370,#7371));
#1552=EDGE_LOOP('',(#7372,#7373,#7374,#7375));
#1553=EDGE_LOOP('',(#7376));
#1554=EDGE_LOOP('',(#7377));
#1555=EDGE_LOOP('',(#7378));
#1556=EDGE_LOOP('',(#7379));
#1557=EDGE_LOOP('',(#7380));
#1558=EDGE_LOOP('',(#7381));
#1559=EDGE_LOOP('',(#7382));
#1560=EDGE_LOOP('',(#7383));
#1561=EDGE_LOOP('',(#7384));
#1562=EDGE_LOOP('',(#7385,#7386,#7387,#7388));
#1563=EDGE_LOOP('',(#7389,#7390,#7391,#7392));
#1564=EDGE_LOOP('',(#7393,#7394,#7395,#7396));
#1565=EDGE_LOOP('',(#7397,#7398,#7399,#7400));
#1566=EDGE_LOOP('',(#7401,#7402,#7403,#7404));
#1567=EDGE_LOOP('',(#7405,#7406,#7407,#7408));
#1568=EDGE_LOOP('',(#7409,#7410,#7411,#7412));
#1569=EDGE_LOOP('',(#7413,#7414,#7415,#7416));
#1570=EDGE_LOOP('',(#7417,#7418,#7419,#7420));
#1571=EDGE_LOOP('',(#7421,#7422,#7423,#7424));
#1572=EDGE_LOOP('',(#7425,#7426,#7427,#7428));
#1573=EDGE_LOOP('',(#7429,#7430,#7431,#7432));
#1574=EDGE_LOOP('',(#7433,#7434,#7435,#7436));
#1575=EDGE_LOOP('',(#7437,#7438,#7439,#7440));
#1576=EDGE_LOOP('',(#7441,#7442,#7443,#7444));
#1577=EDGE_LOOP('',(#7445,#7446,#7447,#7448));
#1578=EDGE_LOOP('',(#7449,#7450,#7451,#7452));
#1579=EDGE_LOOP('',(#7453,#7454,#7455,#7456));
#1580=EDGE_LOOP('',(#7457,#7458,#7459,#7460));
#1581=EDGE_LOOP('',(#7461,#7462,#7463,#7464));
#1582=EDGE_LOOP('',(#7465,#7466,#7467,#7468));
#1583=EDGE_LOOP('',(#7469,#7470,#7471,#7472));
#1584=EDGE_LOOP('',(#7473,#7474,#7475,#7476));
#1585=EDGE_LOOP('',(#7477,#7478,#7479,#7480));
#1586=EDGE_LOOP('',(#7481,#7482,#7483,#7484));
#1587=EDGE_LOOP('',(#7485,#7486,#7487,#7488));
#1588=EDGE_LOOP('',(#7489,#7490,#7491,#7492));
#1589=EDGE_LOOP('',(#7493,#7494,#7495,#7496));
#1590=EDGE_LOOP('',(#7497,#7498,#7499,#7500));
#1591=EDGE_LOOP('',(#7501,#7502,#7503,#7504));
#1592=EDGE_LOOP('',(#7505,#7506,#7507,#7508));
#1593=EDGE_LOOP('',(#7509,#7510,#7511,#7512));
#1594=EDGE_LOOP('',(#7513,#7514,#7515,#7516));
#1595=EDGE_LOOP('',(#7517,#7518,#7519,#7520));
#1596=EDGE_LOOP('',(#7521,#7522,#7523,#7524));
#1597=EDGE_LOOP('',(#7525,#7526,#7527,#7528));
#1598=EDGE_LOOP('',(#7529,#7530,#7531,#7532));
#1599=EDGE_LOOP('',(#7533,#7534,#7535,#7536));
#1600=EDGE_LOOP('',(#7537));
#1601=EDGE_LOOP('',(#7538,#7539,#7540,#7541));
#1602=EDGE_LOOP('',(#7542,#7543,#7544,#7545));
#1603=EDGE_LOOP('',(#7546,#7547,#7548,#7549));
#1604=EDGE_LOOP('',(#7550,#7551,#7552,#7553));
#1605=EDGE_LOOP('',(#7554));
#1606=EDGE_LOOP('',(#7555));
#1607=EDGE_LOOP('',(#7556,#7557,#7558,#7559,#7560,#7561,#7562,#7563,#7564,
#7565,#7566,#7567,#7568,#7569,#7570,#7571,#7572,#7573));
#1608=EDGE_LOOP('',(#7574,#7575,#7576,#7577));
#1609=EDGE_LOOP('',(#7578,#7579,#7580,#7581));
#1610=EDGE_LOOP('',(#7582,#7583,#7584,#7585,#7586,#7587));
#1611=EDGE_LOOP('',(#7588,#7589,#7590));
#1612=EDGE_LOOP('',(#7591,#7592,#7593,#7594,#7595,#7596));
#1613=EDGE_LOOP('',(#7597,#7598,#7599));
#1614=EDGE_LOOP('',(#7600,#7601,#7602,#7603,#7604,#7605));
#1615=EDGE_LOOP('',(#7606,#7607,#7608,#7609));
#1616=EDGE_LOOP('',(#7610,#7611,#7612,#7613));
#1617=EDGE_LOOP('',(#7614,#7615,#7616,#7617));
#1618=EDGE_LOOP('',(#7618,#7619,#7620,#7621,#7622,#7623,#7624,#7625,#7626,
#7627,#7628,#7629,#7630,#7631,#7632,#7633,#7634,#7635,#7636,#7637,#7638,
#7639,#7640,#7641,#7642,#7643,#7644,#7645,#7646,#7647,#7648,#7649,#7650,
#7651,#7652,#7653,#7654,#7655,#7656,#7657));
#1619=EDGE_LOOP('',(#7658));
#1620=EDGE_LOOP('',(#7659));
#1621=EDGE_LOOP('',(#7660));
#1622=EDGE_LOOP('',(#7661));
#1623=EDGE_LOOP('',(#7662));
#1624=EDGE_LOOP('',(#7663));
#1625=EDGE_LOOP('',(#7664,#7665,#7666,#7667));
#1626=EDGE_LOOP('',(#7668,#7669,#7670,#7671));
#1627=EDGE_LOOP('',(#7672,#7673,#7674,#7675));
#1628=EDGE_LOOP('',(#7676,#7677,#7678,#7679));
#1629=EDGE_LOOP('',(#7680,#7681,#7682,#7683));
#1630=EDGE_LOOP('',(#7684,#7685,#7686,#7687));
#1631=EDGE_LOOP('',(#7688,#7689,#7690,#7691,#7692,#7693,#7694,#7695,#7696,
#7697,#7698,#7699,#7700,#7701,#7702,#7703,#7704,#7705,#7706,#7707,#7708,
#7709,#7710,#7711));
#1632=EDGE_LOOP('',(#7712));
#1633=EDGE_LOOP('',(#7713));
#1634=EDGE_LOOP('',(#7714));
#1635=EDGE_LOOP('',(#7715));
#1636=EDGE_LOOP('',(#7716));
#1637=EDGE_LOOP('',(#7717));
#1638=EDGE_LOOP('',(#7718,#7719,#7720,#7721));
#1639=EDGE_LOOP('',(#7722,#7723,#7724,#7725));
#1640=EDGE_LOOP('',(#7726,#7727,#7728,#7729));
#1641=EDGE_LOOP('',(#7730,#7731,#7732,#7733));
#1642=EDGE_LOOP('',(#7734));
#1643=EDGE_LOOP('',(#7735));
#1644=EDGE_LOOP('',(#7736,#7737,#7738,#7739,#7740,#7741,#7742,#7743));
#1645=EDGE_LOOP('',(#7744,#7745,#7746,#7747,#7748,#7749));
#1646=EDGE_LOOP('',(#7750,#7751,#7752,#7753,#7754,#7755,#7756,#7757,#7758,
#7759,#7760,#7761,#7762,#7763,#7764,#7765,#7766,#7767,#7768,#7769,#7770,
#7771,#7772,#7773,#7774,#7775,#7776,#7777,#7778,#7779,#7780,#7781,#7782,
#7783,#7784,#7785,#7786,#7787,#7788,#7789));
#1647=EDGE_LOOP('',(#7790,#7791,#7792,#7793,#7794,#7795));
#1648=EDGE_LOOP('',(#7796,#7797,#7798,#7799,#7800,#7801,#7802,#7803));
#1649=EDGE_LOOP('',(#7804,#7805,#7806,#7807));
#1650=EDGE_LOOP('',(#7808,#7809,#7810,#7811,#7812,#7813,#7814,#7815,#7816,
#7817,#7818,#7819,#7820,#7821,#7822,#7823));
#1651=EDGE_LOOP('',(#7824,#7825,#7826,#7827));
#1652=EDGE_LOOP('',(#7828,#7829,#7830,#7831));
#1653=EDGE_LOOP('',(#7832,#7833,#7834,#7835,#7836,#7837));
#1654=EDGE_LOOP('',(#7838,#7839,#7840,#7841,#7842,#7843,#7844,#7845,#7846,
#7847,#7848,#7849));
#1655=EDGE_LOOP('',(#7850,#7851,#7852,#7853,#7854,#7855));
#1656=EDGE_LOOP('',(#7856,#7857,#7858,#7859));
#1657=EDGE_LOOP('',(#7860,#7861,#7862,#7863));
#1658=EDGE_LOOP('',(#7864,#7865,#7866,#7867,#7868,#7869,#7870,#7871,#7872,
#7873,#7874,#7875,#7876,#7877,#7878,#7879));
#1659=EDGE_LOOP('',(#7880,#7881,#7882,#7883));
#1660=EDGE_LOOP('',(#7884,#7885,#7886,#7887));
#1661=EDGE_LOOP('',(#7888,#7889,#7890,#7891));
#1662=EDGE_LOOP('',(#7892,#7893,#7894,#7895));
#1663=EDGE_LOOP('',(#7896,#7897,#7898,#7899,#7900));
#1664=EDGE_LOOP('',(#7901,#7902,#7903,#7904));
#1665=EDGE_LOOP('',(#7905,#7906,#7907,#7908,#7909,#7910));
#1666=EDGE_LOOP('',(#7911,#7912,#7913,#7914));
#1667=EDGE_LOOP('',(#7915,#7916,#7917,#7918,#7919));
#1668=EDGE_LOOP('',(#7920,#7921,#7922,#7923));
#1669=EDGE_LOOP('',(#7924,#7925,#7926,#7927,#7928));
#1670=EDGE_LOOP('',(#7929,#7930,#7931,#7932));
#1671=EDGE_LOOP('',(#7933,#7934,#7935,#7936,#7937,#7938));
#1672=EDGE_LOOP('',(#7939,#7940,#7941,#7942));
#1673=EDGE_LOOP('',(#7943,#7944,#7945,#7946,#7947));
#1674=EDGE_LOOP('',(#7948,#7949,#7950,#7951));
#1675=EDGE_LOOP('',(#7952,#7953,#7954,#7955,#7956));
#1676=EDGE_LOOP('',(#7957,#7958,#7959,#7960));
#1677=EDGE_LOOP('',(#7961,#7962,#7963,#7964,#7965,#7966));
#1678=EDGE_LOOP('',(#7967,#7968,#7969,#7970));
#1679=EDGE_LOOP('',(#7971,#7972,#7973,#7974,#7975));
#1680=EDGE_LOOP('',(#7976,#7977,#7978,#7979));
#1681=EDGE_LOOP('',(#7980,#7981,#7982,#7983));
#1682=EDGE_LOOP('',(#7984,#7985,#7986,#7987));
#1683=EDGE_LOOP('',(#7988,#7989,#7990,#7991,#7992,#7993,#7994,#7995));
#1684=EDGE_LOOP('',(#7996,#7997,#7998,#7999,#8000,#8001,#8002,#8003,#8004,
#8005,#8006,#8007,#8008,#8009,#8010,#8011));
#1685=EDGE_LOOP('',(#8012));
#1686=EDGE_LOOP('',(#8013,#8014,#8015,#8016,#8017,#8018));
#1687=EDGE_LOOP('',(#8019,#8020,#8021,#8022,#8023,#8024));
#1688=EDGE_LOOP('',(#8025,#8026,#8027,#8028,#8029,#8030,#8031,#8032,#8033,
#8034,#8035,#8036,#8037,#8038,#8039,#8040,#8041,#8042,#8043,#8044,#8045,
#8046,#8047,#8048,#8049,#8050,#8051,#8052,#8053,#8054,#8055,#8056,#8057,
#8058,#8059,#8060,#8061,#8062,#8063,#8064));
#1689=EDGE_LOOP('',(#8065,#8066,#8067,#8068,#8069,#8070,#8071,#8072));
#1690=EDGE_LOOP('',(#8073,#8074,#8075,#8076,#8077,#8078,#8079,#8080,#8081,
#8082,#8083,#8084,#8085,#8086,#8087,#8088));
#1691=EDGE_LOOP('',(#8089,#8090,#8091,#8092));
#1692=EDGE_LOOP('',(#8093,#8094,#8095,#8096));
#1693=EDGE_LOOP('',(#8097,#8098,#8099,#8100,#8101,#8102));
#1694=EDGE_LOOP('',(#8103,#8104,#8105,#8106,#8107,#8108,#8109,#8110,#8111,
#8112,#8113,#8114));
#1695=EDGE_LOOP('',(#8115,#8116,#8117,#8118,#8119,#8120));
#1696=EDGE_LOOP('',(#8121,#8122,#8123,#8124));
#1697=EDGE_LOOP('',(#8125,#8126,#8127,#8128));
#1698=EDGE_LOOP('',(#8129,#8130,#8131,#8132,#8133,#8134,#8135,#8136,#8137,
#8138,#8139,#8140,#8141,#8142,#8143,#8144));
#1699=EDGE_LOOP('',(#8145,#8146,#8147,#8148));
#1700=EDGE_LOOP('',(#8149,#8150,#8151,#8152));
#1701=EDGE_LOOP('',(#8153,#8154,#8155,#8156));
#1702=EDGE_LOOP('',(#8157,#8158,#8159,#8160,#8161));
#1703=EDGE_LOOP('',(#8162,#8163,#8164,#8165));
#1704=EDGE_LOOP('',(#8166,#8167,#8168,#8169));
#1705=EDGE_LOOP('',(#8170,#8171,#8172,#8173,#8174,#8175));
#1706=EDGE_LOOP('',(#8176,#8177,#8178,#8179));
#1707=EDGE_LOOP('',(#8180,#8181,#8182,#8183,#8184,#8185));
#1708=EDGE_LOOP('',(#8186,#8187,#8188,#8189));
#1709=EDGE_LOOP('',(#8190,#8191,#8192));
#1710=EDGE_LOOP('',(#8193,#8194,#8195,#8196,#8197,#8198,#8199,#8200));
#1711=EDGE_LOOP('',(#8201,#8202,#8203,#8204));
#1712=EDGE_LOOP('',(#8205,#8206,#8207,#8208));
#1713=EDGE_LOOP('',(#8209,#8210,#8211,#8212));
#1714=EDGE_LOOP('',(#8213,#8214,#8215,#8216));
#1715=EDGE_LOOP('',(#8217,#8218,#8219,#8220));
#1716=EDGE_LOOP('',(#8221,#8222,#8223,#8224,#8225,#8226,#8227));
#1717=EDGE_LOOP('',(#8228,#8229,#8230));
#1718=EDGE_LOOP('',(#8231,#8232,#8233,#8234,#8235));
#1719=EDGE_LOOP('',(#8236,#8237,#8238,#8239));
#1720=EDGE_LOOP('',(#8240,#8241,#8242,#8243));
#1721=EDGE_LOOP('',(#8244,#8245,#8246,#8247));
#1722=EDGE_LOOP('',(#8248,#8249,#8250,#8251,#8252));
#1723=EDGE_LOOP('',(#8253,#8254,#8255));
#1724=EDGE_LOOP('',(#8256,#8257,#8258,#8259,#8260));
#1725=EDGE_LOOP('',(#8261,#8262,#8263,#8264));
#1726=EDGE_LOOP('',(#8265,#8266,#8267));
#1727=EDGE_LOOP('',(#8268,#8269,#8270,#8271,#8272));
#1728=EDGE_LOOP('',(#8273,#8274,#8275,#8276));
#1729=EDGE_LOOP('',(#8277,#8278,#8279,#8280));
#1730=EDGE_LOOP('',(#8281,#8282,#8283,#8284));
#1731=EDGE_LOOP('',(#8285,#8286,#8287,#8288,#8289));
#1732=EDGE_LOOP('',(#8290,#8291,#8292));
#1733=EDGE_LOOP('',(#8293,#8294,#8295,#8296,#8297));
#1734=EDGE_LOOP('',(#8298,#8299,#8300,#8301));
#1735=EDGE_LOOP('',(#8302,#8303,#8304,#8305,#8306,#8307));
#1736=EDGE_LOOP('',(#8308,#8309,#8310));
#1737=EDGE_LOOP('',(#8311,#8312,#8313,#8314));
#1738=EDGE_LOOP('',(#8315,#8316,#8317,#8318,#8319,#8320));
#1739=EDGE_LOOP('',(#8321));
#1740=EDGE_LOOP('',(#8322,#8323,#8324,#8325,#8326));
#1741=EDGE_LOOP('',(#8327));
#1742=EDGE_LOOP('',(#8328,#8329,#8330,#8331,#8332,#8333,#8334));
#1743=EDGE_LOOP('',(#8335));
#1744=EDGE_LOOP('',(#8336,#8337,#8338,#8339,#8340,#8341));
#1745=EDGE_LOOP('',(#8342));
#1746=EDGE_LOOP('',(#8343,#8344,#8345,#8346,#8347));
#1747=EDGE_LOOP('',(#8348));
#1748=EDGE_LOOP('',(#8349,#8350,#8351,#8352,#8353,#8354,#8355));
#1749=EDGE_LOOP('',(#8356));
#1750=EDGE_LOOP('',(#8357,#8358,#8359,#8360));
#1751=EDGE_LOOP('',(#8361,#8362,#8363,#8364));
#1752=EDGE_LOOP('',(#8365,#8366,#8367,#8368));
#1753=EDGE_LOOP('',(#8369,#8370,#8371,#8372));
#1754=EDGE_LOOP('',(#8373,#8374,#8375,#8376));
#1755=EDGE_LOOP('',(#8377,#8378,#8379,#8380));
#1756=EDGE_LOOP('',(#8381,#8382,#8383,#8384));
#1757=EDGE_LOOP('',(#8385,#8386,#8387,#8388,#8389,#8390,#8391,#8392));
#1758=EDGE_LOOP('',(#8393,#8394,#8395));
#1759=EDGE_LOOP('',(#8396,#8397,#8398,#8399));
#1760=EDGE_LOOP('',(#8400,#8401,#8402,#8403));
#1761=EDGE_LOOP('',(#8404,#8405,#8406,#8407));
#1762=EDGE_LOOP('',(#8408,#8409,#8410,#8411));
#1763=EDGE_LOOP('',(#8412,#8413,#8414,#8415));
#1764=EDGE_LOOP('',(#8416,#8417,#8418,#8419));
#1765=EDGE_LOOP('',(#8420,#8421,#8422,#8423));
#1766=EDGE_LOOP('',(#8424,#8425,#8426,#8427));
#1767=EDGE_LOOP('',(#8428,#8429,#8430,#8431));
#1768=EDGE_LOOP('',(#8432,#8433,#8434,#8435));
#1769=EDGE_LOOP('',(#8436,#8437,#8438,#8439));
#1770=EDGE_LOOP('',(#8440,#8441,#8442,#8443));
#1771=EDGE_LOOP('',(#8444,#8445,#8446,#8447));
#1772=EDGE_LOOP('',(#8448,#8449,#8450,#8451));
#1773=EDGE_LOOP('',(#8452,#8453,#8454,#8455));
#1774=EDGE_LOOP('',(#8456,#8457,#8458,#8459));
#1775=EDGE_LOOP('',(#8460,#8461,#8462,#8463));
#1776=EDGE_LOOP('',(#8464,#8465,#8466,#8467));
#1777=EDGE_LOOP('',(#8468,#8469,#8470,#8471));
#1778=EDGE_LOOP('',(#8472,#8473,#8474,#8475));
#1779=EDGE_LOOP('',(#8476,#8477,#8478,#8479));
#1780=EDGE_LOOP('',(#8480,#8481,#8482,#8483));
#1781=EDGE_LOOP('',(#8484,#8485,#8486,#8487));
#1782=EDGE_LOOP('',(#8488,#8489,#8490,#8491));
#1783=EDGE_LOOP('',(#8492,#8493,#8494,#8495));
#1784=EDGE_LOOP('',(#8496,#8497,#8498,#8499,#8500));
#1785=EDGE_LOOP('',(#8501,#8502,#8503,#8504));
#1786=EDGE_LOOP('',(#8505,#8506,#8507,#8508));
#1787=EDGE_LOOP('',(#8509,#8510,#8511,#8512,#8513,#8514));
#1788=EDGE_LOOP('',(#8515,#8516,#8517,#8518));
#1789=EDGE_LOOP('',(#8519,#8520,#8521,#8522,#8523));
#1790=EDGE_LOOP('',(#8524,#8525,#8526));
#1791=EDGE_LOOP('',(#8527,#8528,#8529,#8530,#8531));
#1792=EDGE_LOOP('',(#8532,#8533,#8534,#8535));
#1793=EDGE_LOOP('',(#8536,#8537,#8538,#8539));
#1794=EDGE_LOOP('',(#8540,#8541,#8542,#8543));
#1795=EDGE_LOOP('',(#8544,#8545,#8546,#8547,#8548));
#1796=EDGE_LOOP('',(#8549,#8550,#8551));
#1797=EDGE_LOOP('',(#8552,#8553,#8554,#8555,#8556));
#1798=EDGE_LOOP('',(#8557,#8558,#8559));
#1799=EDGE_LOOP('',(#8560,#8561,#8562,#8563,#8564));
#1800=EDGE_LOOP('',(#8565,#8566,#8567,#8568,#8569));
#1801=EDGE_LOOP('',(#8570,#8571,#8572));
#1802=EDGE_LOOP('',(#8573,#8574,#8575,#8576,#8577,#8578,#8579));
#1803=EDGE_LOOP('',(#8580,#8581,#8582,#8583));
#1804=EDGE_LOOP('',(#8584,#8585,#8586,#8587));
#1805=EDGE_LOOP('',(#8588,#8589,#8590,#8591));
#1806=EDGE_LOOP('',(#8592,#8593,#8594,#8595));
#1807=EDGE_LOOP('',(#8596,#8597,#8598,#8599));
#1808=EDGE_LOOP('',(#8600,#8601,#8602,#8603));
#1809=EDGE_LOOP('',(#8604,#8605,#8606,#8607,#8608,#8609));
#1810=EDGE_LOOP('',(#8610,#8611,#8612,#8613));
#1811=EDGE_LOOP('',(#8614,#8615,#8616,#8617,#8618,#8619));
#1812=EDGE_LOOP('',(#8620,#8621,#8622,#8623));
#1813=EDGE_LOOP('',(#8624,#8625,#8626));
#1814=EDGE_LOOP('',(#8627,#8628,#8629,#8630));
#1815=EDGE_LOOP('',(#8631,#8632,#8633,#8634,#8635,#8636));
#1816=EDGE_LOOP('',(#8637));
#1817=EDGE_LOOP('',(#8638,#8639,#8640,#8641,#8642));
#1818=EDGE_LOOP('',(#8643));
#1819=EDGE_LOOP('',(#8644,#8645,#8646,#8647,#8648,#8649,#8650));
#1820=EDGE_LOOP('',(#8651));
#1821=EDGE_LOOP('',(#8652,#8653,#8654,#8655,#8656,#8657));
#1822=EDGE_LOOP('',(#8658));
#1823=EDGE_LOOP('',(#8659,#8660,#8661,#8662,#8663));
#1824=EDGE_LOOP('',(#8664));
#1825=EDGE_LOOP('',(#8665,#8666,#8667,#8668,#8669,#8670,#8671));
#1826=EDGE_LOOP('',(#8672));
#1827=EDGE_LOOP('',(#8673,#8674,#8675,#8676));
#1828=EDGE_LOOP('',(#8677,#8678,#8679,#8680));
#1829=EDGE_LOOP('',(#8681,#8682,#8683,#8684));
#1830=EDGE_LOOP('',(#8685,#8686,#8687,#8688));
#1831=EDGE_LOOP('',(#8689,#8690,#8691,#8692));
#1832=EDGE_LOOP('',(#8693,#8694,#8695,#8696));
#1833=EDGE_LOOP('',(#8697,#8698,#8699,#8700));
#1834=EDGE_LOOP('',(#8701,#8702,#8703,#8704));
#1835=EDGE_LOOP('',(#8705,#8706,#8707,#8708));
#1836=EDGE_LOOP('',(#8709,#8710,#8711,#8712));
#1837=EDGE_LOOP('',(#8713,#8714,#8715,#8716));
#1838=EDGE_LOOP('',(#8717));
#1839=EDGE_LOOP('',(#8718));
#1840=EDGE_LOOP('',(#8719,#8720,#8721,#8722,#8723));
#1841=EDGE_LOOP('',(#8724,#8725,#8726,#8727));
#1842=EDGE_LOOP('',(#8728,#8729,#8730,#8731,#8732));
#1843=EDGE_LOOP('',(#8733,#8734,#8735,#8736,#8737,#8738,#8739,#8740,#8741,
#8742,#8743,#8744,#8745,#8746,#8747,#8748,#8749,#8750,#8751,#8752));
#1844=EDGE_LOOP('',(#8753,#8754,#8755,#8756,#8757));
#1845=EDGE_LOOP('',(#8758,#8759,#8760,#8761));
#1846=EDGE_LOOP('',(#8762,#8763,#8764,#8765,#8766,#8767));
#1847=EDGE_LOOP('',(#8768,#8769,#8770,#8771,#8772,#8773,#8774,#8775));
#1848=EDGE_LOOP('',(#8776,#8777,#8778,#8779));
#1849=EDGE_LOOP('',(#8780,#8781,#8782,#8783));
#1850=EDGE_LOOP('',(#8784,#8785,#8786,#8787,#8788));
#1851=EDGE_LOOP('',(#8789,#8790,#8791,#8792,#8793));
#1852=EDGE_LOOP('',(#8794,#8795,#8796,#8797,#8798));
#1853=EDGE_LOOP('',(#8799,#8800,#8801,#8802,#8803));
#1854=EDGE_LOOP('',(#8804,#8805,#8806,#8807,#8808));
#1855=EDGE_LOOP('',(#8809,#8810,#8811,#8812,#8813));
#1856=EDGE_LOOP('',(#8814,#8815,#8816,#8817,#8818));
#1857=EDGE_LOOP('',(#8819,#8820,#8821,#8822));
#1858=EDGE_LOOP('',(#8823,#8824,#8825,#8826,#8827));
#1859=EDGE_LOOP('',(#8828,#8829,#8830,#8831,#8832));
#1860=EDGE_LOOP('',(#8833,#8834,#8835,#8836,#8837));
#1861=EDGE_LOOP('',(#8838,#8839,#8840,#8841,#8842));
#1862=EDGE_LOOP('',(#8843,#8844,#8845,#8846,#8847));
#1863=EDGE_LOOP('',(#8848,#8849,#8850,#8851,#8852));
#1864=EDGE_LOOP('',(#8853,#8854,#8855,#8856,#8857));
#1865=EDGE_LOOP('',(#8858,#8859,#8860,#8861,#8862,#8863));
#1866=EDGE_LOOP('',(#8864,#8865,#8866,#8867,#8868));
#1867=EDGE_LOOP('',(#8869,#8870,#8871,#8872,#8873));
#1868=EDGE_LOOP('',(#8874,#8875,#8876));
#1869=EDGE_LOOP('',(#8877,#8878,#8879));
#1870=EDGE_LOOP('',(#8880,#8881,#8882));
#1871=EDGE_LOOP('',(#8883,#8884,#8885));
#1872=EDGE_LOOP('',(#8886,#8887,#8888));
#1873=EDGE_LOOP('',(#8889,#8890,#8891));
#1874=EDGE_LOOP('',(#8892));
#1875=EDGE_LOOP('',(#8893));
#1876=EDGE_LOOP('',(#8894,#8895,#8896,#8897,#8898));
#1877=EDGE_LOOP('',(#8899,#8900,#8901,#8902,#8903));
#1878=EDGE_LOOP('',(#8904,#8905,#8906,#8907,#8908));
#1879=EDGE_LOOP('',(#8909,#8910,#8911,#8912,#8913));
#1880=EDGE_LOOP('',(#8914,#8915,#8916,#8917,#8918,#8919,#8920,#8921));
#1881=EDGE_LOOP('',(#8922,#8923,#8924,#8925));
#1882=EDGE_LOOP('',(#8926,#8927,#8928,#8929));
#1883=EDGE_LOOP('',(#8930,#8931,#8932,#8933));
#1884=EDGE_LOOP('',(#8934,#8935,#8936,#8937,#8938));
#1885=EDGE_LOOP('',(#8939,#8940,#8941,#8942,#8943));
#1886=EDGE_LOOP('',(#8944,#8945,#8946,#8947,#8948));
#1887=EDGE_LOOP('',(#8949,#8950,#8951,#8952,#8953));
#1888=EDGE_LOOP('',(#8954,#8955,#8956,#8957,#8958));
#1889=EDGE_LOOP('',(#8959,#8960,#8961));
#1890=EDGE_LOOP('',(#8962,#8963,#8964));
#1891=EDGE_LOOP('',(#8965,#8966,#8967));
#1892=EDGE_LOOP('',(#8968,#8969,#8970));
#1893=EDGE_LOOP('',(#8971,#8972,#8973,#8974));
#1894=EDGE_LOOP('',(#8975,#8976,#8977,#8978));
#1895=EDGE_LOOP('',(#8979,#8980,#8981,#8982));
#1896=EDGE_LOOP('',(#8983,#8984,#8985,#8986));
#1897=EDGE_LOOP('',(#8987,#8988,#8989,#8990));
#1898=EDGE_LOOP('',(#8991,#8992,#8993,#8994));
#1899=EDGE_LOOP('',(#8995,#8996,#8997,#8998));
#1900=EDGE_LOOP('',(#8999,#9000,#9001,#9002));
#1901=EDGE_LOOP('',(#9003,#9004,#9005,#9006));
#1902=EDGE_LOOP('',(#9007,#9008,#9009,#9010));
#1903=EDGE_LOOP('',(#9011,#9012,#9013,#9014));
#1904=EDGE_LOOP('',(#9015,#9016,#9017,#9018));
#1905=EDGE_LOOP('',(#9019,#9020,#9021,#9022));
#1906=EDGE_LOOP('',(#9023,#9024,#9025,#9026));
#1907=EDGE_LOOP('',(#9027));
#1908=EDGE_LOOP('',(#9028,#9029,#9030,#9031));
#1909=EDGE_LOOP('',(#9032));
#1910=EDGE_LOOP('',(#9033));
#1911=EDGE_LOOP('',(#9034,#9035,#9036,#9037));
#1912=EDGE_LOOP('',(#9038));
#1913=EDGE_LOOP('',(#9039));
#1914=EDGE_LOOP('',(#9040));
#1915=EDGE_LOOP('',(#9041));
#1916=EDGE_LOOP('',(#9042));
#1917=EDGE_LOOP('',(#9043));
#1918=EDGE_LOOP('',(#9044));
#1919=EDGE_LOOP('',(#9045,#9046,#9047,#9048));
#1920=EDGE_LOOP('',(#9049,#9050,#9051,#9052));
#1921=EDGE_LOOP('',(#9053,#9054,#9055,#9056));
#1922=EDGE_LOOP('',(#9057,#9058,#9059,#9060));
#1923=EDGE_LOOP('',(#9061,#9062,#9063,#9064));
#1924=EDGE_LOOP('',(#9065,#9066,#9067,#9068));
#1925=EDGE_LOOP('',(#9069,#9070,#9071,#9072));
#1926=EDGE_LOOP('',(#9073,#9074,#9075,#9076));
#1927=EDGE_LOOP('',(#9077,#9078,#9079,#9080));
#1928=EDGE_LOOP('',(#9081,#9082,#9083,#9084));
#1929=EDGE_LOOP('',(#9085,#9086,#9087,#9088));
#1930=EDGE_LOOP('',(#9089,#9090,#9091,#9092));
#1931=EDGE_LOOP('',(#9093,#9094,#9095,#9096));
#1932=EDGE_LOOP('',(#9097,#9098,#9099,#9100));
#1933=EDGE_LOOP('',(#9101,#9102,#9103,#9104));
#1934=EDGE_LOOP('',(#9105,#9106,#9107,#9108));
#1935=EDGE_LOOP('',(#9109,#9110,#9111,#9112));
#1936=EDGE_LOOP('',(#9113,#9114,#9115,#9116));
#1937=EDGE_LOOP('',(#9117,#9118,#9119,#9120));
#1938=EDGE_LOOP('',(#9121,#9122,#9123,#9124));
#1939=EDGE_LOOP('',(#9125,#9126,#9127,#9128));
#1940=EDGE_LOOP('',(#9129,#9130,#9131,#9132));
#1941=EDGE_LOOP('',(#9133,#9134,#9135,#9136));
#1942=EDGE_LOOP('',(#9137,#9138,#9139,#9140));
#1943=EDGE_LOOP('',(#9141,#9142,#9143,#9144));
#1944=EDGE_LOOP('',(#9145,#9146,#9147,#9148));
#1945=EDGE_LOOP('',(#9149,#9150,#9151,#9152));
#1946=EDGE_LOOP('',(#9153,#9154,#9155,#9156));
#1947=EDGE_LOOP('',(#9157,#9158,#9159,#9160));
#1948=EDGE_LOOP('',(#9161,#9162,#9163,#9164));
#1949=EDGE_LOOP('',(#9165,#9166,#9167,#9168));
#1950=EDGE_LOOP('',(#9169,#9170,#9171,#9172));
#1951=EDGE_LOOP('',(#9173,#9174,#9175,#9176));
#1952=EDGE_LOOP('',(#9177,#9178,#9179,#9180));
#1953=EDGE_LOOP('',(#9181,#9182,#9183,#9184));
#1954=EDGE_LOOP('',(#9185,#9186,#9187,#9188));
#1955=EDGE_LOOP('',(#9189,#9190,#9191,#9192));
#1956=EDGE_LOOP('',(#9193,#9194,#9195,#9196));
#1957=EDGE_LOOP('',(#9197,#9198,#9199,#9200));
#1958=EDGE_LOOP('',(#9201,#9202,#9203,#9204));
#1959=EDGE_LOOP('',(#9205,#9206,#9207,#9208));
#1960=EDGE_LOOP('',(#9209,#9210,#9211,#9212));
#1961=EDGE_LOOP('',(#9213,#9214,#9215,#9216,#9217,#9218));
#1962=EDGE_LOOP('',(#9219));
#1963=EDGE_LOOP('',(#9220));
#1964=EDGE_LOOP('',(#9221));
#1965=EDGE_LOOP('',(#9222));
#1966=EDGE_LOOP('',(#9223));
#1967=EDGE_LOOP('',(#9224));
#1968=EDGE_LOOP('',(#9225));
#1969=EDGE_LOOP('',(#9226));
#1970=EDGE_LOOP('',(#9227));
#1971=EDGE_LOOP('',(#9228));
#1972=EDGE_LOOP('',(#9229));
#1973=EDGE_LOOP('',(#9230));
#1974=EDGE_LOOP('',(#9231));
#1975=EDGE_LOOP('',(#9232));
#1976=EDGE_LOOP('',(#9233));
#1977=EDGE_LOOP('',(#9234));
#1978=EDGE_LOOP('',(#9235));
#1979=EDGE_LOOP('',(#9236));
#1980=EDGE_LOOP('',(#9237));
#1981=EDGE_LOOP('',(#9238));
#1982=EDGE_LOOP('',(#9239));
#1983=EDGE_LOOP('',(#9240));
#1984=EDGE_LOOP('',(#9241));
#1985=EDGE_LOOP('',(#9242));
#1986=EDGE_LOOP('',(#9243));
#1987=EDGE_LOOP('',(#9244,#9245,#9246,#9247,#9248));
#1988=EDGE_LOOP('',(#9249,#9250,#9251,#9252,#9253,#9254,#9255,#9256,#9257,
#9258,#9259,#9260));
#1989=EDGE_LOOP('',(#9261,#9262,#9263,#9264,#9265));
#1990=EDGE_LOOP('',(#9266,#9267,#9268,#9269,#9270));
#1991=EDGE_LOOP('',(#9271,#9272,#9273,#9274));
#1992=EDGE_LOOP('',(#9275,#9276,#9277,#9278,#9279));
#1993=EDGE_LOOP('',(#9280,#9281,#9282,#9283,#9284,#9285));
#1994=EDGE_LOOP('',(#9286));
#1995=EDGE_LOOP('',(#9287));
#1996=EDGE_LOOP('',(#9288));
#1997=EDGE_LOOP('',(#9289));
#1998=EDGE_LOOP('',(#9290));
#1999=EDGE_LOOP('',(#9291));
#2000=EDGE_LOOP('',(#9292));
#2001=EDGE_LOOP('',(#9293));
#2002=EDGE_LOOP('',(#9294));
#2003=EDGE_LOOP('',(#9295));
#2004=EDGE_LOOP('',(#9296));
#2005=EDGE_LOOP('',(#9297));
#2006=EDGE_LOOP('',(#9298));
#2007=EDGE_LOOP('',(#9299));
#2008=EDGE_LOOP('',(#9300));
#2009=EDGE_LOOP('',(#9301));
#2010=EDGE_LOOP('',(#9302));
#2011=EDGE_LOOP('',(#9303));
#2012=EDGE_LOOP('',(#9304));
#2013=EDGE_LOOP('',(#9305));
#2014=EDGE_LOOP('',(#9306));
#2015=EDGE_LOOP('',(#9307));
#2016=EDGE_LOOP('',(#9308));
#2017=EDGE_LOOP('',(#9309));
#2018=EDGE_LOOP('',(#9310));
#2019=EDGE_LOOP('',(#9311,#9312,#9313,#9314,#9315,#9316,#9317,#9318));
#2020=EDGE_LOOP('',(#9319));
#2021=EDGE_LOOP('',(#9320));
#2022=EDGE_LOOP('',(#9321));
#2023=EDGE_LOOP('',(#9322));
#2024=EDGE_LOOP('',(#9323,#9324,#9325,#9326,#9327));
#2025=EDGE_LOOP('',(#9328,#9329,#9330,#9331,#9332));
#2026=EDGE_LOOP('',(#9333,#9334,#9335,#9336,#9337,#9338,#9339,#9340));
#2027=EDGE_LOOP('',(#9341));
#2028=EDGE_LOOP('',(#9342));
#2029=EDGE_LOOP('',(#9343));
#2030=EDGE_LOOP('',(#9344));
#2031=EDGE_LOOP('',(#9345,#9346,#9347,#9348,#9349));
#2032=EDGE_LOOP('',(#9350,#9351,#9352,#9353,#9354));
#2033=EDGE_LOOP('',(#9355,#9356,#9357,#9358,#9359));
#2034=EDGE_LOOP('',(#9360,#9361,#9362,#9363));
#2035=EDGE_LOOP('',(#9364,#9365,#9366,#9367));
#2036=EDGE_LOOP('',(#9368,#9369,#9370,#9371));
#2037=EDGE_LOOP('',(#9372,#9373,#9374,#9375));
#2038=EDGE_LOOP('',(#9376,#9377,#9378,#9379,#9380));
#2039=EDGE_LOOP('',(#9381,#9382,#9383,#9384,#9385));
#2040=EDGE_LOOP('',(#9386,#9387,#9388,#9389));
#2041=EDGE_LOOP('',(#9390,#9391,#9392,#9393));
#2042=EDGE_LOOP('',(#9394,#9395,#9396,#9397));
#2043=EDGE_LOOP('',(#9398,#9399,#9400,#9401,#9402));
#2044=EDGE_LOOP('',(#9403,#9404,#9405,#9406));
#2045=EDGE_LOOP('',(#9407,#9408,#9409,#9410,#9411,#9412,#9413,#9414));
#2046=EDGE_LOOP('',(#9415));
#2047=EDGE_LOOP('',(#9416));
#2048=EDGE_LOOP('',(#9417));
#2049=EDGE_LOOP('',(#9418));
#2050=EDGE_LOOP('',(#9419,#9420,#9421,#9422,#9423,#9424,#9425,#9426));
#2051=EDGE_LOOP('',(#9427));
#2052=EDGE_LOOP('',(#9428));
#2053=EDGE_LOOP('',(#9429));
#2054=EDGE_LOOP('',(#9430));
#2055=EDGE_LOOP('',(#9431,#9432,#9433,#9434));
#2056=EDGE_LOOP('',(#9435,#9436,#9437,#9438));
#2057=EDGE_LOOP('',(#9439,#9440,#9441,#9442));
#2058=EDGE_LOOP('',(#9443,#9444,#9445,#9446));
#2059=EDGE_LOOP('',(#9447,#9448,#9449,#9450));
#2060=EDGE_LOOP('',(#9451,#9452,#9453,#9454));
#2061=EDGE_LOOP('',(#9455,#9456,#9457,#9458));
#2062=EDGE_LOOP('',(#9459,#9460,#9461,#9462));
#2063=EDGE_LOOP('',(#9463,#9464,#9465,#9466));
#2064=EDGE_LOOP('',(#9467,#9468,#9469,#9470));
#2065=EDGE_LOOP('',(#9471,#9472,#9473,#9474,#9475));
#2066=EDGE_LOOP('',(#9476,#9477,#9478,#9479));
#2067=EDGE_LOOP('',(#9480,#9481,#9482,#9483));
#2068=EDGE_LOOP('',(#9484,#9485,#9486,#9487));
#2069=EDGE_LOOP('',(#9488,#9489,#9490,#9491));
#2070=EDGE_LOOP('',(#9492,#9493,#9494,#9495));
#2071=EDGE_LOOP('',(#9496,#9497,#9498,#9499));
#2072=EDGE_LOOP('',(#9500,#9501,#9502,#9503));
#2073=EDGE_LOOP('',(#9504,#9505,#9506,#9507));
#2074=EDGE_LOOP('',(#9508,#9509,#9510,#9511));
#2075=EDGE_LOOP('',(#9512,#9513,#9514,#9515,#9516));
#2076=EDGE_LOOP('',(#9517,#9518,#9519,#9520));
#2077=EDGE_LOOP('',(#9521));
#2078=EDGE_LOOP('',(#9522));
#2079=EDGE_LOOP('',(#9523));
#2080=EDGE_LOOP('',(#9524));
#2081=EDGE_LOOP('',(#9525));
#2082=EDGE_LOOP('',(#9526));
#2083=EDGE_LOOP('',(#9527));
#2084=EDGE_LOOP('',(#9528));
#2085=EDGE_LOOP('',(#9529));
#2086=EDGE_LOOP('',(#9530));
#2087=EDGE_LOOP('',(#9531,#9532,#9533,#9534));
#2088=EDGE_LOOP('',(#9535));
#2089=EDGE_LOOP('',(#9536));
#2090=EDGE_LOOP('',(#9537));
#2091=EDGE_LOOP('',(#9538));
#2092=EDGE_LOOP('',(#9539));
#2093=EDGE_LOOP('',(#9540));
#2094=EDGE_LOOP('',(#9541));
#2095=EDGE_LOOP('',(#9542));
#2096=EDGE_LOOP('',(#9543));
#2097=EDGE_LOOP('',(#9544));
#2098=EDGE_LOOP('',(#9545,#9546,#9547,#9548));
#2099=EDGE_LOOP('',(#9549,#9550,#9551,#9552));
#2100=EDGE_LOOP('',(#9553,#9554,#9555,#9556));
#2101=EDGE_LOOP('',(#9557,#9558,#9559,#9560));
#2102=EDGE_LOOP('',(#9561,#9562,#9563,#9564));
#2103=EDGE_LOOP('',(#9565,#9566,#9567,#9568));
#2104=EDGE_LOOP('',(#9569,#9570,#9571,#9572));
#2105=EDGE_LOOP('',(#9573,#9574,#9575,#9576));
#2106=EDGE_LOOP('',(#9577,#9578,#9579,#9580));
#2107=EDGE_LOOP('',(#9581,#9582,#9583,#9584));
#2108=EDGE_LOOP('',(#9585,#9586,#9587,#9588,#9589,#9590,#9591,#9592,#9593,
#9594));
#2109=EDGE_LOOP('',(#9595));
#2110=EDGE_LOOP('',(#9596));
#2111=EDGE_LOOP('',(#9597));
#2112=EDGE_LOOP('',(#9598,#9599,#9600,#9601));
#2113=EDGE_LOOP('',(#9602,#9603,#9604,#9605));
#2114=EDGE_LOOP('',(#9606,#9607,#9608,#9609));
#2115=EDGE_LOOP('',(#9610,#9611,#9612,#9613));
#2116=EDGE_LOOP('',(#9614,#9615,#9616,#9617,#9618,#9619,#9620,#9621,#9622,
#9623));
#2117=EDGE_LOOP('',(#9624));
#2118=EDGE_LOOP('',(#9625));
#2119=EDGE_LOOP('',(#9626));
#2120=EDGE_LOOP('',(#9627,#9628,#9629,#9630));
#2121=EDGE_LOOP('',(#9631,#9632,#9633,#9634));
#2122=EDGE_LOOP('',(#9635,#9636,#9637,#9638));
#2123=EDGE_LOOP('',(#9639,#9640,#9641,#9642));
#2124=EDGE_LOOP('',(#9643,#9644,#9645,#9646,#9647,#9648,#9649,#9650,#9651,
#9652,#9653));
#2125=EDGE_LOOP('',(#9654));
#2126=EDGE_LOOP('',(#9655));
#2127=EDGE_LOOP('',(#9656,#9657,#9658,#9659,#9660,#9661,#9662,#9663,#9664,
#9665,#9666));
#2128=EDGE_LOOP('',(#9667));
#2129=EDGE_LOOP('',(#9668));
#2130=EDGE_LOOP('',(#9669,#9670,#9671,#9672));
#2131=EDGE_LOOP('',(#9673,#9674,#9675,#9676));
#2132=EDGE_LOOP('',(#9677,#9678,#9679,#9680));
#2133=EDGE_LOOP('',(#9681,#9682,#9683,#9684));
#2134=EDGE_LOOP('',(#9685,#9686,#9687,#9688));
#2135=EDGE_LOOP('',(#9689,#9690,#9691,#9692));
#2136=EDGE_LOOP('',(#9693,#9694,#9695,#9696));
#2137=EDGE_LOOP('',(#9697,#9698,#9699,#9700));
#2138=EDGE_LOOP('',(#9701,#9702,#9703,#9704));
#2139=EDGE_LOOP('',(#9705,#9706,#9707,#9708));
#2140=EDGE_LOOP('',(#9709,#9710,#9711,#9712));
#2141=EDGE_LOOP('',(#9713,#9714,#9715,#9716));
#2142=EDGE_LOOP('',(#9717,#9718,#9719,#9720));
#2143=EDGE_LOOP('',(#9721,#9722,#9723,#9724));
#2144=EDGE_LOOP('',(#9725,#9726,#9727,#9728));
#2145=EDGE_LOOP('',(#9729,#9730,#9731,#9732));
#2146=EDGE_LOOP('',(#9733,#9734,#9735,#9736));
#2147=EDGE_LOOP('',(#9737,#9738,#9739,#9740));
#2148=EDGE_LOOP('',(#9741,#9742,#9743,#9744,#9745,#9746));
#2149=EDGE_LOOP('',(#9747));
#2150=EDGE_LOOP('',(#9748));
#2151=EDGE_LOOP('',(#9749,#9750,#9751,#9752));
#2152=EDGE_LOOP('',(#9753,#9754,#9755,#9756,#9757,#9758));
#2153=EDGE_LOOP('',(#9759));
#2154=EDGE_LOOP('',(#9760));
#2155=EDGE_LOOP('',(#9761,#9762,#9763,#9764));
#2156=EDGE_LOOP('',(#9765,#9766,#9767,#9768,#9769,#9770));
#2157=EDGE_LOOP('',(#9771));
#2158=EDGE_LOOP('',(#9772));
#2159=EDGE_LOOP('',(#9773,#9774,#9775,#9776,#9777,#9778));
#2160=EDGE_LOOP('',(#9779));
#2161=EDGE_LOOP('',(#9780));
#2162=EDGE_LOOP('',(#9781,#9782,#9783,#9784,#9785,#9786,#9787,#9788,#9789,
#9790,#9791,#9792));
#2163=EDGE_LOOP('',(#9793,#9794,#9795,#9796,#9797,#9798,#9799,#9800,#9801,
#9802,#9803,#9804));
#2164=EDGE_LOOP('',(#9805,#9806,#9807,#9808));
#2165=EDGE_LOOP('',(#9809,#9810,#9811,#9812));
#2166=EDGE_LOOP('',(#9813,#9814,#9815,#9816));
#2167=EDGE_LOOP('',(#9817,#9818,#9819,#9820));
#2168=EDGE_LOOP('',(#9821,#9822,#9823,#9824));
#2169=EDGE_LOOP('',(#9825,#9826,#9827,#9828));
#2170=EDGE_LOOP('',(#9829,#9830,#9831,#9832));
#2171=EDGE_LOOP('',(#9833,#9834,#9835,#9836));
#2172=EDGE_LOOP('',(#9837,#9838,#9839,#9840));
#2173=EDGE_LOOP('',(#9841,#9842,#9843,#9844,#9845,#9846));
#2174=EDGE_LOOP('',(#9847));
#2175=EDGE_LOOP('',(#9848,#9849,#9850,#9851));
#2176=EDGE_LOOP('',(#9852,#9853,#9854,#9855,#9856,#9857));
#2177=EDGE_LOOP('',(#9858));
#2178=EDGE_LOOP('',(#9859,#9860,#9861,#9862));
#2179=EDGE_LOOP('',(#9863,#9864,#9865,#9866));
#2180=EDGE_LOOP('',(#9867,#9868,#9869,#9870));
#2181=EDGE_LOOP('',(#9871,#9872,#9873,#9874));
#2182=EDGE_LOOP('',(#9875,#9876,#9877,#9878));
#2183=EDGE_LOOP('',(#9879,#9880,#9881,#9882,#9883));
#2184=EDGE_LOOP('',(#9884,#9885,#9886,#9887,#9888));
#2185=EDGE_LOOP('',(#9889,#9890,#9891,#9892));
#2186=EDGE_LOOP('',(#9893,#9894,#9895,#9896));
#2187=EDGE_LOOP('',(#9897));
#2188=EDGE_LOOP('',(#9898));
#2189=EDGE_LOOP('',(#9899));
#2190=EDGE_LOOP('',(#9900));
#2191=EDGE_LOOP('',(#9901,#9902));
#2192=EDGE_LOOP('',(#9903,#9904));
#2193=EDGE_LOOP('',(#9905,#9906));
#2194=EDGE_LOOP('',(#9907,#9908));
#2195=EDGE_LOOP('',(#9909,#9910));
#2196=EDGE_LOOP('',(#9911,#9912));
#2197=EDGE_LOOP('',(#9913,#9914));
#2198=EDGE_LOOP('',(#9915,#9916));
#2199=EDGE_LOOP('',(#9917,#9918));
#2200=EDGE_LOOP('',(#9919,#9920));
#2201=EDGE_LOOP('',(#9921,#9922));
#2202=EDGE_LOOP('',(#9923,#9924));
#2203=EDGE_LOOP('',(#9925,#9926,#9927,#9928));
#2204=EDGE_LOOP('',(#9929,#9930,#9931,#9932));
#2205=EDGE_LOOP('',(#9933));
#2206=EDGE_LOOP('',(#9934));
#2207=EDGE_LOOP('',(#9935));
#2208=EDGE_LOOP('',(#9936));
#2209=EDGE_LOOP('',(#9937,#9938,#9939,#9940));
#2210=EDGE_LOOP('',(#9941,#9942,#9943,#9944));
#2211=EDGE_LOOP('',(#9945));
#2212=EDGE_LOOP('',(#9946));
#2213=EDGE_LOOP('',(#9947));
#2214=EDGE_LOOP('',(#9948));
#2215=EDGE_LOOP('',(#9949,#9950,#9951,#9952));
#2216=EDGE_LOOP('',(#9953,#9954,#9955,#9956));
#2217=EDGE_LOOP('',(#9957,#9958,#9959,#9960));
#2218=EDGE_LOOP('',(#9961,#9962,#9963,#9964));
#2219=EDGE_LOOP('',(#9965,#9966,#9967,#9968,#9969));
#2220=EDGE_LOOP('',(#9970,#9971,#9972,#9973,#9974));
#2221=EDGE_LOOP('',(#9975));
#2222=EDGE_LOOP('',(#9976));
#2223=EDGE_LOOP('',(#9977));
#2224=EDGE_LOOP('',(#9978));
#2225=EDGE_LOOP('',(#9979));
#2226=EDGE_LOOP('',(#9980));
#2227=EDGE_LOOP('',(#9981,#9982,#9983,#9984));
#2228=EDGE_LOOP('',(#9985,#9986,#9987,#9988));
#2229=EDGE_LOOP('',(#9989,#9990,#9991,#9992));
#2230=EDGE_LOOP('',(#9993));
#2231=EDGE_LOOP('',(#9994));
#2232=EDGE_LOOP('',(#9995));
#2233=EDGE_LOOP('',(#9996));
#2234=EDGE_LOOP('',(#9997));
#2235=EDGE_LOOP('',(#9998));
#2236=EDGE_LOOP('',(#9999,#10000,#10001,#10002));
#2237=EDGE_LOOP('',(#10003,#10004,#10005,#10006));
#2238=EDGE_LOOP('',(#10007,#10008,#10009,#10010));
#2239=EDGE_LOOP('',(#10011));
#2240=EDGE_LOOP('',(#10012));
#2241=EDGE_LOOP('',(#10013));
#2242=EDGE_LOOP('',(#10014));
#2243=EDGE_LOOP('',(#10015));
#2244=EDGE_LOOP('',(#10016));
#2245=EDGE_LOOP('',(#10017,#10018,#10019,#10020));
#2246=EDGE_LOOP('',(#10021,#10022,#10023,#10024));
#2247=EDGE_LOOP('',(#10025,#10026,#10027,#10028));
#2248=EDGE_LOOP('',(#10029,#10030,#10031,#10032));
#2249=EDGE_LOOP('',(#10033,#10034,#10035,#10036));
#2250=EDGE_LOOP('',(#10037,#10038,#10039,#10040));
#2251=EDGE_LOOP('',(#10041));
#2252=EDGE_LOOP('',(#10042));
#2253=EDGE_LOOP('',(#10043,#10044,#10045,#10046));
#2254=EDGE_LOOP('',(#10047));
#2255=EDGE_LOOP('',(#10048));
#2256=EDGE_LOOP('',(#10049,#10050,#10051,#10052));
#2257=EDGE_LOOP('',(#10053,#10054,#10055,#10056));
#2258=EDGE_LOOP('',(#10057,#10058,#10059,#10060));
#2259=EDGE_LOOP('',(#10061,#10062,#10063,#10064,#10065,#10066,#10067,#10068));
#2260=EDGE_LOOP('',(#10069,#10070,#10071,#10072));
#2261=EDGE_LOOP('',(#10073,#10074,#10075,#10076));
#2262=EDGE_LOOP('',(#10077,#10078,#10079,#10080));
#2263=EDGE_LOOP('',(#10081,#10082,#10083,#10084));
#2264=EDGE_LOOP('',(#10085,#10086,#10087,#10088));
#2265=EDGE_LOOP('',(#10089));
#2266=EDGE_LOOP('',(#10090,#10091,#10092,#10093,#10094,#10095));
#2267=EDGE_LOOP('',(#10096));
#2268=EDGE_LOOP('',(#10097,#10098,#10099,#10100,#10101));
#2269=EDGE_LOOP('',(#10102,#10103,#10104,#10105,#10106));
#2270=EDGE_LOOP('',(#10107,#10108,#10109,#10110,#10111));
#2271=EDGE_LOOP('',(#10112,#10113,#10114,#10115,#10116));
#2272=EDGE_LOOP('',(#10117,#10118,#10119,#10120,#10121));
#2273=EDGE_LOOP('',(#10122,#10123,#10124,#10125,#10126));
#2274=EDGE_LOOP('',(#10127,#10128,#10129));
#2275=EDGE_LOOP('',(#10130,#10131,#10132));
#2276=EDGE_LOOP('',(#10133,#10134,#10135));
#2277=EDGE_LOOP('',(#10136,#10137,#10138));
#2278=EDGE_LOOP('',(#10139,#10140,#10141));
#2279=EDGE_LOOP('',(#10142,#10143,#10144));
#2280=LINE('',#15428,#3268);
#2281=LINE('',#15434,#3269);
#2282=LINE('',#15440,#3270);
#2283=LINE('',#15446,#3271);
#2284=LINE('',#15452,#3272);
#2285=LINE('',#15458,#3273);
#2286=LINE('',#15464,#3274);
#2287=LINE('',#15470,#3275);
#2288=LINE('',#15476,#3276);
#2289=LINE('',#15482,#3277);
#2290=LINE('',#15488,#3278);
#2291=LINE('',#15494,#3279);
#2292=LINE('',#15500,#3280);
#2293=LINE('',#15506,#3281);
#2294=LINE('',#15512,#3282);
#2295=LINE('',#15518,#3283);
#2296=LINE('',#15524,#3284);
#2297=LINE('',#15529,#3285);
#2298=LINE('',#15533,#3286);
#2299=LINE('',#15537,#3287);
#2300=LINE('',#15539,#3288);
#2301=LINE('',#15540,#3289);
#2302=LINE('',#15544,#3290);
#2303=LINE('',#15548,#3291);
#2304=LINE('',#15552,#3292);
#2305=LINE('',#15554,#3293);
#2306=LINE('',#15555,#3294);
#2307=LINE('',#15559,#3295);
#2308=LINE('',#15564,#3296);
#2309=LINE('',#15566,#3297);
#2310=LINE('',#15567,#3298);
#2311=LINE('',#15571,#3299);
#2312=LINE('',#15575,#3300);
#2313=LINE('',#15578,#3301);
#2314=LINE('',#15579,#3302);
#2315=LINE('',#15583,#3303);
#2316=LINE('',#15585,#3304);
#2317=LINE('',#15587,#3305);
#2318=LINE('',#15591,#3306);
#2319=LINE('',#15595,#3307);
#2320=LINE('',#15600,#3308);
#2321=LINE('',#15601,#3309);
#2322=LINE('',#15602,#3310);
#2323=LINE('',#15607,#3311);
#2324=LINE('',#15612,#3312);
#2325=LINE('',#15615,#3313);
#2326=LINE('',#15616,#3314);
#2327=LINE('',#15618,#3315);
#2328=LINE('',#15620,#3316);
#2329=LINE('',#15622,#3317);
#2330=LINE('',#15627,#3318);
#2331=LINE('',#15631,#3319);
#2332=LINE('',#15635,#3320);
#2333=LINE('',#15638,#3321);
#2334=LINE('',#15641,#3322);
#2335=LINE('',#15643,#3323);
#2336=LINE('',#15644,#3324);
#2337=LINE('',#15648,#3325);
#2338=LINE('',#15650,#3326);
#2339=LINE('',#15652,#3327);
#2340=LINE('',#15656,#3328);
#2341=LINE('',#15660,#3329);
#2342=LINE('',#15662,#3330);
#2343=LINE('',#15665,#3331);
#2344=LINE('',#15667,#3332);
#2345=LINE('',#15669,#3333);
#2346=LINE('',#15670,#3334);
#2347=LINE('',#15672,#3335);
#2348=LINE('',#15673,#3336);
#2349=LINE('',#15675,#3337);
#2350=LINE('',#15676,#3338);
#2351=LINE('',#15678,#3339);
#2352=LINE('',#15679,#3340);
#2353=LINE('',#15693,#3341);
#2354=LINE('',#15699,#3342);
#2355=LINE('',#15705,#3343);
#2356=LINE('',#15711,#3344);
#2357=LINE('',#15717,#3345);
#2358=LINE('',#15723,#3346);
#2359=LINE('',#15729,#3347);
#2360=LINE('',#15735,#3348);
#2361=LINE('',#15741,#3349);
#2362=LINE('',#15747,#3350);
#2363=LINE('',#15753,#3351);
#2364=LINE('',#15759,#3352);
#2365=LINE('',#15765,#3353);
#2366=LINE('',#15771,#3354);
#2367=LINE('',#15777,#3355);
#2368=LINE('',#15783,#3356);
#2369=LINE('',#15789,#3357);
#2370=LINE('',#15795,#3358);
#2371=LINE('',#15801,#3359);
#2372=LINE('',#15807,#3360);
#2373=LINE('',#15813,#3361);
#2374=LINE('',#15819,#3362);
#2375=LINE('',#15824,#3363);
#2376=LINE('',#15826,#3364);
#2377=LINE('',#15828,#3365);
#2378=LINE('',#15829,#3366);
#2379=LINE('',#15834,#3367);
#2380=LINE('',#15839,#3368);
#2381=LINE('',#15845,#3369);
#2382=LINE('',#15852,#3370);
#2383=LINE('',#15857,#3371);
#2384=LINE('',#15859,#3372);
#2385=LINE('',#15861,#3373);
#2386=LINE('',#15863,#3374);
#2387=LINE('',#15865,#3375);
#2388=LINE('',#15867,#3376);
#2389=LINE('',#15869,#3377);
#2390=LINE('',#15871,#3378);
#2391=LINE('',#15873,#3379);
#2392=LINE('',#15875,#3380);
#2393=LINE('',#15877,#3381);
#2394=LINE('',#15879,#3382);
#2395=LINE('',#15881,#3383);
#2396=LINE('',#15883,#3384);
#2397=LINE('',#15885,#3385);
#2398=LINE('',#15887,#3386);
#2399=LINE('',#15888,#3387);
#2400=LINE('',#15928,#3388);
#2401=LINE('',#15930,#3389);
#2402=LINE('',#15931,#3390);
#2403=LINE('',#16121,#3391);
#2404=LINE('',#16180,#3392);
#2405=LINE('',#16181,#3393);
#2406=LINE('',#16239,#3394);
#2407=LINE('',#16241,#3395);
#2408=LINE('',#16243,#3396);
#2409=LINE('',#16299,#3397);
#2410=LINE('',#16305,#3398);
#2411=LINE('',#16311,#3399);
#2412=LINE('',#16317,#3400);
#2413=LINE('',#16321,#3401);
#2414=LINE('',#16325,#3402);
#2415=LINE('',#16329,#3403);
#2416=LINE('',#16333,#3404);
#2417=LINE('',#16336,#3405);
#2418=LINE('',#16340,#3406);
#2419=LINE('',#16344,#3407);
#2420=LINE('',#16348,#3408);
#2421=LINE('',#16352,#3409);
#2422=LINE('',#16356,#3410);
#2423=LINE('',#16360,#3411);
#2424=LINE('',#16364,#3412);
#2425=LINE('',#16368,#3413);
#2426=LINE('',#16372,#3414);
#2427=LINE('',#16376,#3415);
#2428=LINE('',#16380,#3416);
#2429=LINE('',#16385,#3417);
#2430=LINE('',#16392,#3418);
#2431=LINE('',#16396,#3419);
#2432=LINE('',#16401,#3420);
#2433=LINE('',#16407,#3421);
#2434=LINE('',#16418,#3422);
#2435=LINE('',#16421,#3423);
#2436=LINE('',#16425,#3424);
#2437=LINE('',#16429,#3425);
#2438=LINE('',#16433,#3426);
#2439=LINE('',#16437,#3427);
#2440=LINE('',#16440,#3428);
#2441=LINE('',#16537,#3429);
#2442=LINE('',#16539,#3430);
#2443=LINE('',#16540,#3431);
#2444=LINE('',#16542,#3432);
#2445=LINE('',#16544,#3433);
#2446=LINE('',#16545,#3434);
#2447=LINE('',#16548,#3435);
#2448=LINE('',#16549,#3436);
#2449=LINE('',#16553,#3437);
#2450=LINE('',#16555,#3438);
#2451=LINE('',#16557,#3439);
#2452=LINE('',#16559,#3440);
#2453=LINE('',#16561,#3441);
#2454=LINE('',#16563,#3442);
#2455=LINE('',#16565,#3443);
#2456=LINE('',#16567,#3444);
#2457=LINE('',#16569,#3445);
#2458=LINE('',#16571,#3446);
#2459=LINE('',#16573,#3447);
#2460=LINE('',#16575,#3448);
#2461=LINE('',#16577,#3449);
#2462=LINE('',#16579,#3450);
#2463=LINE('',#16580,#3451);
#2464=LINE('',#16582,#3452);
#2465=LINE('',#16584,#3453);
#2466=LINE('',#16586,#3454);
#2467=LINE('',#16588,#3455);
#2468=LINE('',#16590,#3456);
#2469=LINE('',#16592,#3457);
#2470=LINE('',#16594,#3458);
#2471=LINE('',#16596,#3459);
#2472=LINE('',#16598,#3460);
#2473=LINE('',#16600,#3461);
#2474=LINE('',#16602,#3462);
#2475=LINE('',#16604,#3463);
#2476=LINE('',#16606,#3464);
#2477=LINE('',#16608,#3465);
#2478=LINE('',#16610,#3466);
#2479=LINE('',#16612,#3467);
#2480=LINE('',#16614,#3468);
#2481=LINE('',#16616,#3469);
#2482=LINE('',#16618,#3470);
#2483=LINE('',#16620,#3471);
#2484=LINE('',#16622,#3472);
#2485=LINE('',#16624,#3473);
#2486=LINE('',#16625,#3474);
#2487=LINE('',#16628,#3475);
#2488=LINE('',#16629,#3476);
#2489=LINE('',#16633,#3477);
#2490=LINE('',#16635,#3478);
#2491=LINE('',#16637,#3479);
#2492=LINE('',#16638,#3480);
#2493=LINE('',#16639,#3481);
#2494=LINE('',#16642,#3482);
#2495=LINE('',#16645,#3483);
#2496=LINE('',#16648,#3484);
#2497=LINE('',#16650,#3485);
#2498=LINE('',#16652,#3486);
#2499=LINE('',#16654,#3487);
#2500=LINE('',#16656,#3488);
#2501=LINE('',#16658,#3489);
#2502=LINE('',#16660,#3490);
#2503=LINE('',#16662,#3491);
#2504=LINE('',#16664,#3492);
#2505=LINE('',#16666,#3493);
#2506=LINE('',#16668,#3494);
#2507=LINE('',#16670,#3495);
#2508=LINE('',#16672,#3496);
#2509=LINE('',#16673,#3497);
#2510=LINE('',#16677,#3498);
#2511=LINE('',#16680,#3499);
#2512=LINE('',#16681,#3500);
#2513=LINE('',#16688,#3501);
#2514=LINE('',#16692,#3502);
#2515=LINE('',#16694,#3503);
#2516=LINE('',#16696,#3504);
#2517=LINE('',#16698,#3505);
#2518=LINE('',#16700,#3506);
#2519=LINE('',#16702,#3507);
#2520=LINE('',#16704,#3508);
#2521=LINE('',#16706,#3509);
#2522=LINE('',#16708,#3510);
#2523=LINE('',#16709,#3511);
#2524=LINE('',#16715,#3512);
#2525=LINE('',#16719,#3513);
#2526=LINE('',#16720,#3514);
#2527=LINE('',#16724,#3515);
#2528=LINE('',#16727,#3516);
#2529=LINE('',#16729,#3517);
#2530=LINE('',#16731,#3518);
#2531=LINE('',#16733,#3519);
#2532=LINE('',#16735,#3520);
#2533=LINE('',#16737,#3521);
#2534=LINE('',#16739,#3522);
#2535=LINE('',#16741,#3523);
#2536=LINE('',#16743,#3524);
#2537=LINE('',#16745,#3525);
#2538=LINE('',#16747,#3526);
#2539=LINE('',#16749,#3527);
#2540=LINE('',#16751,#3528);
#2541=LINE('',#16752,#3529);
#2542=LINE('',#16761,#3530);
#2543=LINE('',#16762,#3531);
#2544=LINE('',#16765,#3532);
#2545=LINE('',#16774,#3533);
#2546=LINE('',#16775,#3534);
#2547=LINE('',#16779,#3535);
#2548=LINE('',#16787,#3536);
#2549=LINE('',#16793,#3537);
#2550=LINE('',#16797,#3538);
#2551=LINE('',#16800,#3539);
#2552=LINE('',#16806,#3540);
#2553=LINE('',#16809,#3541);
#2554=LINE('',#16818,#3542);
#2555=LINE('',#16819,#3543);
#2556=LINE('',#16823,#3544);
#2557=LINE('',#16831,#3545);
#2558=LINE('',#16837,#3546);
#2559=LINE('',#16841,#3547);
#2560=LINE('',#16844,#3548);
#2561=LINE('',#16850,#3549);
#2562=LINE('',#16853,#3550);
#2563=LINE('',#16862,#3551);
#2564=LINE('',#16863,#3552);
#2565=LINE('',#16867,#3553);
#2566=LINE('',#16875,#3554);
#2567=LINE('',#16881,#3555);
#2568=LINE('',#16885,#3556);
#2569=LINE('',#16888,#3557);
#2570=LINE('',#16894,#3558);
#2571=LINE('',#16897,#3559);
#2572=LINE('',#16901,#3560);
#2573=LINE('',#16907,#3561);
#2574=LINE('',#16909,#3562);
#2575=LINE('',#16911,#3563);
#2576=LINE('',#16913,#3564);
#2577=LINE('',#16914,#3565);
#2578=LINE('',#16920,#3566);
#2579=LINE('',#16922,#3567);
#2580=LINE('',#16924,#3568);
#2581=LINE('',#16928,#3569);
#2582=LINE('',#16930,#3570);
#2583=LINE('',#16932,#3571);
#2584=LINE('',#16936,#3572);
#2585=LINE('',#16938,#3573);
#2586=LINE('',#16940,#3574);
#2587=LINE('',#16943,#3575);
#2588=LINE('',#16944,#3576);
#2589=LINE('',#16947,#3577);
#2590=LINE('',#16948,#3578);
#2591=LINE('',#16951,#3579);
#2592=LINE('',#16953,#3580);
#2593=LINE('',#16954,#3581);
#2594=LINE('',#16958,#3582);
#2595=LINE('',#16960,#3583);
#2596=LINE('',#16962,#3584);
#2597=LINE('',#16964,#3585);
#2598=LINE('',#16966,#3586);
#2599=LINE('',#16968,#3587);
#2600=LINE('',#16970,#3588);
#2601=LINE('',#16972,#3589);
#2602=LINE('',#16973,#3590);
#2603=LINE('',#16975,#3591);
#2604=LINE('',#16977,#3592);
#2605=LINE('',#16979,#3593);
#2606=LINE('',#16981,#3594);
#2607=LINE('',#16983,#3595);
#2608=LINE('',#16985,#3596);
#2609=LINE('',#16987,#3597);
#2610=LINE('',#16989,#3598);
#2611=LINE('',#16991,#3599);
#2612=LINE('',#16993,#3600);
#2613=LINE('',#16995,#3601);
#2614=LINE('',#16997,#3602);
#2615=LINE('',#16999,#3603);
#2616=LINE('',#17001,#3604);
#2617=LINE('',#17003,#3605);
#2618=LINE('',#17005,#3606);
#2619=LINE('',#17007,#3607);
#2620=LINE('',#17008,#3608);
#2621=LINE('',#17010,#3609);
#2622=LINE('',#17012,#3610);
#2623=LINE('',#17014,#3611);
#2624=LINE('',#17016,#3612);
#2625=LINE('',#17018,#3613);
#2626=LINE('',#17020,#3614);
#2627=LINE('',#17022,#3615);
#2628=LINE('',#17024,#3616);
#2629=LINE('',#17026,#3617);
#2630=LINE('',#17027,#3618);
#2631=LINE('',#17030,#3619);
#2632=LINE('',#17032,#3620);
#2633=LINE('',#17034,#3621);
#2634=LINE('',#17036,#3622);
#2635=LINE('',#17037,#3623);
#2636=LINE('',#17041,#3624);
#2637=LINE('',#17043,#3625);
#2638=LINE('',#17044,#3626);
#2639=LINE('',#17046,#3627);
#2640=LINE('',#17048,#3628);
#2641=LINE('',#17050,#3629);
#2642=LINE('',#17052,#3630);
#2643=LINE('',#17054,#3631);
#2644=LINE('',#17056,#3632);
#2645=LINE('',#17058,#3633);
#2646=LINE('',#17060,#3634);
#2647=LINE('',#17062,#3635);
#2648=LINE('',#17064,#3636);
#2649=LINE('',#17066,#3637);
#2650=LINE('',#17067,#3638);
#2651=LINE('',#17070,#3639);
#2652=LINE('',#17074,#3640);
#2653=LINE('',#17075,#3641);
#2654=LINE('',#17078,#3642);
#2655=LINE('',#17086,#3643);
#2656=LINE('',#17087,#3644);
#2657=LINE('',#17089,#3645);
#2658=LINE('',#17091,#3646);
#2659=LINE('',#17093,#3647);
#2660=LINE('',#17095,#3648);
#2661=LINE('',#17097,#3649);
#2662=LINE('',#17099,#3650);
#2663=LINE('',#17101,#3651);
#2664=LINE('',#17102,#3652);
#2665=LINE('',#17105,#3653);
#2666=LINE('',#17112,#3654);
#2667=LINE('',#17113,#3655);
#2668=LINE('',#17116,#3656);
#2669=LINE('',#17121,#3657);
#2670=LINE('',#17122,#3658);
#2671=LINE('',#17124,#3659);
#2672=LINE('',#17126,#3660);
#2673=LINE('',#17128,#3661);
#2674=LINE('',#17130,#3662);
#2675=LINE('',#17132,#3663);
#2676=LINE('',#17134,#3664);
#2677=LINE('',#17136,#3665);
#2678=LINE('',#17138,#3666);
#2679=LINE('',#17140,#3667);
#2680=LINE('',#17142,#3668);
#2681=LINE('',#17144,#3669);
#2682=LINE('',#17145,#3670);
#2683=LINE('',#17152,#3671);
#2684=LINE('',#17154,#3672);
#2685=LINE('',#17155,#3673);
#2686=LINE('',#17157,#3674);
#2687=LINE('',#17158,#3675);
#2688=LINE('',#17162,#3676);
#2689=LINE('',#17163,#3677);
#2690=LINE('',#17164,#3678);
#2691=LINE('',#17168,#3679);
#2692=LINE('',#17169,#3680);
#2693=LINE('',#17172,#3681);
#2694=LINE('',#17175,#3682);
#2695=LINE('',#17179,#3683);
#2696=LINE('',#17181,#3684);
#2697=LINE('',#17183,#3685);
#2698=LINE('',#17184,#3686);
#2699=LINE('',#17186,#3687);
#2700=LINE('',#17187,#3688);
#2701=LINE('',#17191,#3689);
#2702=LINE('',#17193,#3690);
#2703=LINE('',#17194,#3691);
#2704=LINE('',#17197,#3692);
#2705=LINE('',#17198,#3693);
#2706=LINE('',#17201,#3694);
#2707=LINE('',#17203,#3695);
#2708=LINE('',#17204,#3696);
#2709=LINE('',#17207,#3697);
#2710=LINE('',#17208,#3698);
#2711=LINE('',#17211,#3699);
#2712=LINE('',#17212,#3700);
#2713=LINE('',#17216,#3701);
#2714=LINE('',#17217,#3702);
#2715=LINE('',#17218,#3703);
#2716=LINE('',#17221,#3704);
#2717=LINE('',#17222,#3705);
#2718=LINE('',#17224,#3706);
#2719=LINE('',#17225,#3707);
#2720=LINE('',#17228,#3708);
#2721=LINE('',#17229,#3709);
#2722=LINE('',#17231,#3710);
#2723=LINE('',#17233,#3711);
#2724=LINE('',#17234,#3712);
#2725=LINE('',#17236,#3713);
#2726=LINE('',#17238,#3714);
#2727=LINE('',#17240,#3715);
#2728=LINE('',#17243,#3716);
#2729=LINE('',#17244,#3717);
#2730=LINE('',#17247,#3718);
#2731=LINE('',#17248,#3719);
#2732=LINE('',#17250,#3720);
#2733=LINE('',#17252,#3721);
#2734=LINE('',#17253,#3722);
#2735=LINE('',#17257,#3723);
#2736=LINE('',#17258,#3724);
#2737=LINE('',#17260,#3725);
#2738=LINE('',#17262,#3726);
#2739=LINE('',#17263,#3727);
#2740=LINE('',#17265,#3728);
#2741=LINE('',#17267,#3729);
#2742=LINE('',#17269,#3730);
#2743=LINE('',#17272,#3731);
#2744=LINE('',#17273,#3732);
#2745=LINE('',#17276,#3733);
#2746=LINE('',#17277,#3734);
#2747=LINE('',#17279,#3735);
#2748=LINE('',#17281,#3736);
#2749=LINE('',#17282,#3737);
#2750=LINE('',#17284,#3738);
#2751=LINE('',#17289,#3739);
#2752=LINE('',#17290,#3740);
#2753=LINE('',#17293,#3741);
#2754=LINE('',#17295,#3742);
#2755=LINE('',#17297,#3743);
#2756=LINE('',#17298,#3744);
#2757=LINE('',#17301,#3745);
#2758=LINE('',#17303,#3746);
#2759=LINE('',#17305,#3747);
#2760=LINE('',#17306,#3748);
#2761=LINE('',#17309,#3749);
#2762=LINE('',#17311,#3750);
#2763=LINE('',#17313,#3751);
#2764=LINE('',#17314,#3752);
#2765=LINE('',#17317,#3753);
#2766=LINE('',#17319,#3754);
#2767=LINE('',#17321,#3755);
#2768=LINE('',#17322,#3756);
#2769=LINE('',#17325,#3757);
#2770=LINE('',#17327,#3758);
#2771=LINE('',#17329,#3759);
#2772=LINE('',#17330,#3760);
#2773=LINE('',#17333,#3761);
#2774=LINE('',#17335,#3762);
#2775=LINE('',#17336,#3763);
#2776=LINE('',#17339,#3764);
#2777=LINE('',#17340,#3765);
#2778=LINE('',#17342,#3766);
#2779=LINE('',#17343,#3767);
#2780=LINE('',#17345,#3768);
#2781=LINE('',#17347,#3769);
#2782=LINE('',#17350,#3770);
#2783=LINE('',#17351,#3771);
#2784=LINE('',#17354,#3772);
#2785=LINE('',#17355,#3773);
#2786=LINE('',#17358,#3774);
#2787=LINE('',#17360,#3775);
#2788=LINE('',#17361,#3776);
#2789=LINE('',#17364,#3777);
#2790=LINE('',#17365,#3778);
#2791=LINE('',#17367,#3779);
#2792=LINE('',#17370,#3780);
#2793=LINE('',#17371,#3781);
#2794=LINE('',#17374,#3782);
#2795=LINE('',#17376,#3783);
#2796=LINE('',#17377,#3784);
#2797=LINE('',#17380,#3785);
#2798=LINE('',#17381,#3786);
#2799=LINE('',#17384,#3787);
#2800=LINE('',#17385,#3788);
#2801=LINE('',#17388,#3789);
#2802=LINE('',#17389,#3790);
#2803=LINE('',#17391,#3791);
#2804=LINE('',#17393,#3792);
#2805=LINE('',#17395,#3793);
#2806=LINE('',#17397,#3794);
#2807=LINE('',#17434,#3795);
#2808=LINE('',#17437,#3796);
#2809=LINE('',#17438,#3797);
#2810=LINE('',#17440,#3798);
#2811=LINE('',#17442,#3799);
#2812=LINE('',#17444,#3800);
#2813=LINE('',#17446,#3801);
#2814=LINE('',#17449,#3802);
#2815=LINE('',#17450,#3803);
#2816=LINE('',#17453,#3804);
#2817=LINE('',#17454,#3805);
#2818=LINE('',#17456,#3806);
#2819=LINE('',#17458,#3807);
#2820=LINE('',#17459,#3808);
#2821=LINE('',#17461,#3809);
#2822=LINE('',#17463,#3810);
#2823=LINE('',#17465,#3811);
#2824=LINE('',#17468,#3812);
#2825=LINE('',#17469,#3813);
#2826=LINE('',#17472,#3814);
#2827=LINE('',#17473,#3815);
#2828=LINE('',#17476,#3816);
#2829=LINE('',#17477,#3817);
#2830=LINE('',#17480,#3818);
#2831=LINE('',#17481,#3819);
#2832=LINE('',#17483,#3820);
#2833=LINE('',#17485,#3821);
#2834=LINE('',#17488,#3822);
#2835=LINE('',#17489,#3823);
#2836=LINE('',#17491,#3824);
#2837=LINE('',#17493,#3825);
#2838=LINE('',#17494,#3826);
#2839=LINE('',#17497,#3827);
#2840=LINE('',#17498,#3828);
#2841=LINE('',#17501,#3829);
#2842=LINE('',#17503,#3830);
#2843=LINE('',#17504,#3831);
#2844=LINE('',#17507,#3832);
#2845=LINE('',#17508,#3833);
#2846=LINE('',#17511,#3834);
#2847=LINE('',#17512,#3835);
#2848=LINE('',#17515,#3836);
#2849=LINE('',#17516,#3837);
#2850=LINE('',#17519,#3838);
#2851=LINE('',#17520,#3839);
#2852=LINE('',#17525,#3840);
#2853=LINE('',#17527,#3841);
#2854=LINE('',#17528,#3842);
#2855=LINE('',#17532,#3843);
#2856=LINE('',#17535,#3844);
#2857=LINE('',#17537,#3845);
#2858=LINE('',#17539,#3846);
#2859=LINE('',#17540,#3847);
#2860=LINE('',#17542,#3848);
#2861=LINE('',#17543,#3849);
#2862=LINE('',#17547,#3850);
#2863=LINE('',#17548,#3851);
#2864=LINE('',#17551,#3852);
#2865=LINE('',#17553,#3853);
#2866=LINE('',#17555,#3854);
#2867=LINE('',#17556,#3855);
#2868=LINE('',#17560,#3856);
#2869=LINE('',#17561,#3857);
#2870=LINE('',#17563,#3858);
#2871=LINE('',#17564,#3859);
#2872=LINE('',#17567,#3860);
#2873=LINE('',#17569,#3861);
#2874=LINE('',#17570,#3862);
#2875=LINE('',#17573,#3863);
#2876=LINE('',#17575,#3864);
#2877=LINE('',#17577,#3865);
#2878=LINE('',#17578,#3866);
#2879=LINE('',#17582,#3867);
#2880=LINE('',#17583,#3868);
#2881=LINE('',#17585,#3869);
#2882=LINE('',#17586,#3870);
#2883=LINE('',#17589,#3871);
#2884=LINE('',#17591,#3872);
#2885=LINE('',#17592,#3873);
#2886=LINE('',#17594,#3874);
#2887=LINE('',#17596,#3875);
#2888=LINE('',#17598,#3876);
#2889=LINE('',#17601,#3877);
#2890=LINE('',#17602,#3878);
#2891=LINE('',#17605,#3879);
#2892=LINE('',#17607,#3880);
#2893=LINE('',#17608,#3881);
#2894=LINE('',#17611,#3882);
#2895=LINE('',#17612,#3883);
#2896=LINE('',#17615,#3884);
#2897=LINE('',#17616,#3885);
#2898=LINE('',#17619,#3886);
#2899=LINE('',#17620,#3887);
#2900=LINE('',#17622,#3888);
#2901=LINE('',#17624,#3889);
#2902=LINE('',#17626,#3890);
#2903=LINE('',#17629,#3891);
#2904=LINE('',#17631,#3892);
#2905=LINE('',#17634,#3893);
#2906=LINE('',#17635,#3894);
#2907=LINE('',#17638,#3895);
#2908=LINE('',#17640,#3896);
#2909=LINE('',#17641,#3897);
#2910=LINE('',#17643,#3898);
#2911=LINE('',#17644,#3899);
#2912=LINE('',#17646,#3900);
#2913=LINE('',#17647,#3901);
#2914=LINE('',#17648,#3902);
#2915=LINE('',#17651,#3903);
#2916=LINE('',#17652,#3904);
#2917=LINE('',#17653,#3905);
#2918=LINE('',#17656,#3906);
#2919=LINE('',#17658,#3907);
#2920=LINE('',#17661,#3908);
#2921=LINE('',#17663,#3909);
#2922=LINE('',#17665,#3910);
#2923=LINE('',#17666,#3911);
#2924=LINE('',#17669,#3912);
#2925=LINE('',#17672,#3913);
#2926=LINE('',#17676,#3914);
#2927=LINE('',#17679,#3915);
#2928=LINE('',#17682,#3916);
#2929=LINE('',#17683,#3917);
#2930=LINE('',#17685,#3918);
#2931=LINE('',#17686,#3919);
#2932=LINE('',#17688,#3920);
#2933=LINE('',#17691,#3921);
#2934=LINE('',#17694,#3922);
#2935=LINE('',#17695,#3923);
#2936=LINE('',#17697,#3924);
#2937=LINE('',#18413,#3925);
#2938=LINE('',#18416,#3926);
#2939=LINE('',#18419,#3927);
#2940=LINE('',#18422,#3928);
#2941=LINE('',#18424,#3929);
#2942=LINE('',#18426,#3930);
#2943=LINE('',#18427,#3931);
#2944=LINE('',#18430,#3932);
#2945=LINE('',#18433,#3933);
#2946=LINE('',#18434,#3934);
#2947=LINE('',#18436,#3935);
#2948=LINE('',#18437,#3936);
#2949=LINE('',#18439,#3937);
#2950=LINE('',#18440,#3938);
#2951=LINE('',#18450,#3939);
#2952=LINE('',#18451,#3940);
#2953=LINE('',#18452,#3941);
#2954=LINE('',#18455,#3942);
#2955=LINE('',#18456,#3943);
#2956=LINE('',#18459,#3944);
#2957=LINE('',#18460,#3945);
#2958=LINE('',#18462,#3946);
#2959=LINE('',#18730,#3947);
#2960=LINE('',#18731,#3948);
#2961=LINE('',#18732,#3949);
#2962=LINE('',#18735,#3950);
#2963=LINE('',#18736,#3951);
#2964=LINE('',#18739,#3952);
#2965=LINE('',#18740,#3953);
#2966=LINE('',#18742,#3954);
#2967=LINE('',#18756,#3955);
#2968=LINE('',#18762,#3956);
#2969=LINE('',#18768,#3957);
#2970=LINE('',#18774,#3958);
#2971=LINE('',#18780,#3959);
#2972=LINE('',#18786,#3960);
#2973=LINE('',#18792,#3961);
#2974=LINE('',#18798,#3962);
#2975=LINE('',#18804,#3963);
#2976=LINE('',#18810,#3964);
#2977=LINE('',#18816,#3965);
#2978=LINE('',#18822,#3966);
#2979=LINE('',#18828,#3967);
#2980=LINE('',#18834,#3968);
#2981=LINE('',#18840,#3969);
#2982=LINE('',#18846,#3970);
#2983=LINE('',#18852,#3971);
#2984=LINE('',#18858,#3972);
#2985=LINE('',#18864,#3973);
#2986=LINE('',#18870,#3974);
#2987=LINE('',#18876,#3975);
#2988=LINE('',#18882,#3976);
#2989=LINE('',#18888,#3977);
#2990=LINE('',#18894,#3978);
#2991=LINE('',#18900,#3979);
#2992=LINE('',#18904,#3980);
#2993=LINE('',#18908,#3981);
#2994=LINE('',#18912,#3982);
#2995=LINE('',#18916,#3983);
#2996=LINE('',#18920,#3984);
#2997=LINE('',#18924,#3985);
#2998=LINE('',#18928,#3986);
#2999=LINE('',#18932,#3987);
#3000=LINE('',#18936,#3988);
#3001=LINE('',#18942,#3989);
#3002=LINE('',#18948,#3990);
#3003=LINE('',#18954,#3991);
#3004=LINE('',#18960,#3992);
#3005=LINE('',#18966,#3993);
#3006=LINE('',#18972,#3994);
#3007=LINE('',#18978,#3995);
#3008=LINE('',#18984,#3996);
#3009=LINE('',#18989,#3997);
#3010=LINE('',#18991,#3998);
#3011=LINE('',#18995,#3999);
#3012=LINE('',#18998,#4000);
#3013=LINE('',#19019,#4001);
#3014=LINE('',#19022,#4002);
#3015=LINE('',#19024,#4003);
#3016=LINE('',#19026,#4004);
#3017=LINE('',#19030,#4005);
#3018=LINE('',#19034,#4006);
#3019=LINE('',#19036,#4007);
#3020=LINE('',#19038,#4008);
#3021=LINE('',#19042,#4009);
#3022=LINE('',#19061,#4010);
#3023=LINE('',#19063,#4011);
#3024=LINE('',#19066,#4012);
#3025=LINE('',#19069,#4013);
#3026=LINE('',#19070,#4014);
#3027=LINE('',#19075,#4015);
#3028=LINE('',#19076,#4016);
#3029=LINE('',#19078,#4017);
#3030=LINE('',#19079,#4018);
#3031=LINE('',#19082,#4019);
#3032=LINE('',#19086,#4020);
#3033=LINE('',#19090,#4021);
#3034=LINE('',#19143,#4022);
#3035=LINE('',#19181,#4023);
#3036=LINE('',#19201,#4024);
#3037=LINE('',#19204,#4025);
#3038=LINE('',#19207,#4026);
#3039=LINE('',#19210,#4027);
#3040=LINE('',#19215,#4028);
#3041=LINE('',#19218,#4029);
#3042=LINE('',#19219,#4030);
#3043=LINE('',#19221,#4031);
#3044=LINE('',#19222,#4032);
#3045=LINE('',#19226,#4033);
#3046=LINE('',#19229,#4034);
#3047=LINE('',#19232,#4035);
#3048=LINE('',#19235,#4036);
#3049=LINE('',#19236,#4037);
#3050=LINE('',#19288,#4038);
#3051=LINE('',#19289,#4039);
#3052=LINE('',#19292,#4040);
#3053=LINE('',#19294,#4041);
#3054=LINE('',#19295,#4042);
#3055=LINE('',#19299,#4043);
#3056=LINE('',#19302,#4044);
#3057=LINE('',#19305,#4045);
#3058=LINE('',#19307,#4046);
#3059=LINE('',#19311,#4047);
#3060=LINE('',#19313,#4048);
#3061=LINE('',#19320,#4049);
#3062=LINE('',#19326,#4050);
#3063=LINE('',#19332,#4051);
#3064=LINE('',#19338,#4052);
#3065=LINE('',#19344,#4053);
#3066=LINE('',#19350,#4054);
#3067=LINE('',#19356,#4055);
#3068=LINE('',#19362,#4056);
#3069=LINE('',#19370,#4057);
#3070=LINE('',#19377,#4058);
#3071=LINE('',#19383,#4059);
#3072=LINE('',#19389,#4060);
#3073=LINE('',#19395,#4061);
#3074=LINE('',#19401,#4062);
#3075=LINE('',#19407,#4063);
#3076=LINE('',#19413,#4064);
#3077=LINE('',#19419,#4065);
#3078=LINE('',#19425,#4066);
#3079=LINE('',#19429,#4067);
#3080=LINE('',#19434,#4068);
#3081=LINE('',#19438,#4069);
#3082=LINE('',#19445,#4070);
#3083=LINE('',#19448,#4071);
#3084=LINE('',#19450,#4072);
#3085=LINE('',#19451,#4073);
#3086=LINE('',#19453,#4074);
#3087=LINE('',#19454,#4075);
#3088=LINE('',#19463,#4076);
#3089=LINE('',#19469,#4077);
#3090=LINE('',#19475,#4078);
#3091=LINE('',#19482,#4079);
#3092=LINE('',#19485,#4080);
#3093=LINE('',#19490,#4081);
#3094=LINE('',#19496,#4082);
#3095=LINE('',#19501,#4083);
#3096=LINE('',#19503,#4084);
#3097=LINE('',#19505,#4085);
#3098=LINE('',#19507,#4086);
#3099=LINE('',#19509,#4087);
#3100=LINE('',#19511,#4088);
#3101=LINE('',#19513,#4089);
#3102=LINE('',#19515,#4090);
#3103=LINE('',#19517,#4091);
#3104=LINE('',#19518,#4092);
#3105=LINE('',#19521,#4093);
#3106=LINE('',#19523,#4094);
#3107=LINE('',#19524,#4095);
#3108=LINE('',#19527,#4096);
#3109=LINE('',#19529,#4097);
#3110=LINE('',#19530,#4098);
#3111=LINE('',#19534,#4099);
#3112=LINE('',#19536,#4100);
#3113=LINE('',#19538,#4101);
#3114=LINE('',#19539,#4102);
#3115=LINE('',#19542,#4103);
#3116=LINE('',#19544,#4104);
#3117=LINE('',#19545,#4105);
#3118=LINE('',#19548,#4106);
#3119=LINE('',#19550,#4107);
#3120=LINE('',#19552,#4108);
#3121=LINE('',#19554,#4109);
#3122=LINE('',#19555,#4110);
#3123=LINE('',#19556,#4111);
#3124=LINE('',#19557,#4112);
#3125=LINE('',#19561,#4113);
#3126=LINE('',#19563,#4114);
#3127=LINE('',#19565,#4115);
#3128=LINE('',#19566,#4116);
#3129=LINE('',#19575,#4117);
#3130=LINE('',#19577,#4118);
#3131=LINE('',#19581,#4119);
#3132=LINE('',#19584,#4120);
#3133=LINE('',#19590,#4121);
#3134=LINE('',#19597,#4122);
#3135=LINE('',#19599,#4123);
#3136=LINE('',#19601,#4124);
#3137=LINE('',#19602,#4125);
#3138=LINE('',#19605,#4126);
#3139=LINE('',#19607,#4127);
#3140=LINE('',#19608,#4128);
#3141=LINE('',#19611,#4129);
#3142=LINE('',#19613,#4130);
#3143=LINE('',#19614,#4131);
#3144=LINE('',#19616,#4132);
#3145=LINE('',#19617,#4133);
#3146=LINE('',#19626,#4134);
#3147=LINE('',#19632,#4135);
#3148=LINE('',#19638,#4136);
#3149=LINE('',#19644,#4137);
#3150=LINE('',#19650,#4138);
#3151=LINE('',#19655,#4139);
#3152=LINE('',#19657,#4140);
#3153=LINE('',#19659,#4141);
#3154=LINE('',#19660,#4142);
#3155=LINE('',#19664,#4143);
#3156=LINE('',#19665,#4144);
#3157=LINE('',#19667,#4145);
#3158=LINE('',#19669,#4146);
#3159=LINE('',#19670,#4147);
#3160=LINE('',#19673,#4148);
#3161=LINE('',#19675,#4149);
#3162=LINE('',#19676,#4150);
#3163=LINE('',#19680,#4151);
#3164=LINE('',#19682,#4152);
#3165=LINE('',#19683,#4153);
#3166=LINE('',#19685,#4154);
#3167=LINE('',#19686,#4155);
#3168=LINE('',#19690,#4156);
#3169=LINE('',#19691,#4157);
#3170=LINE('',#19692,#4158);
#3171=LINE('',#19696,#4159);
#3172=LINE('',#19698,#4160);
#3173=LINE('',#19700,#4161);
#3174=LINE('',#19701,#4162);
#3175=LINE('',#19702,#4163);
#3176=LINE('',#19706,#4164);
#3177=LINE('',#19708,#4165);
#3178=LINE('',#19710,#4166);
#3179=LINE('',#19711,#4167);
#3180=LINE('',#19712,#4168);
#3181=LINE('',#19715,#4169);
#3182=LINE('',#19717,#4170);
#3183=LINE('',#19719,#4171);
#3184=LINE('',#19721,#4172);
#3185=LINE('',#19722,#4173);
#3186=LINE('',#19723,#4174);
#3187=LINE('',#19724,#4175);
#3188=LINE('',#19728,#4176);
#3189=LINE('',#19729,#4177);
#3190=LINE('',#19730,#4178);
#3191=LINE('',#19731,#4179);
#3192=LINE('',#19733,#4180);
#3193=LINE('',#19735,#4181);
#3194=LINE('',#19736,#4182);
#3195=LINE('',#19746,#4183);
#3196=LINE('',#19749,#4184);
#3197=LINE('',#19752,#4185);
#3198=LINE('',#19754,#4186);
#3199=LINE('',#19755,#4187);
#3200=LINE('',#19758,#4188);
#3201=LINE('',#19760,#4189);
#3202=LINE('',#19761,#4190);
#3203=LINE('',#19769,#4191);
#3204=LINE('',#19771,#4192);
#3205=LINE('',#19773,#4193);
#3206=LINE('',#19775,#4194);
#3207=LINE('',#19789,#4195);
#3208=LINE('',#19796,#4196);
#3209=LINE('',#19799,#4197);
#3210=LINE('',#19803,#4198);
#3211=LINE('',#19808,#4199);
#3212=LINE('',#19863,#4200);
#3213=LINE('',#19869,#4201);
#3214=LINE('',#19877,#4202);
#3215=LINE('',#19883,#4203);
#3216=LINE('',#19891,#4204);
#3217=LINE('',#19897,#4205);
#3218=LINE('',#19906,#4206);
#3219=LINE('',#19913,#4207);
#3220=LINE('',#19917,#4208);
#3221=LINE('',#19927,#4209);
#3222=LINE('',#19933,#4210);
#3223=LINE('',#19939,#4211);
#3224=LINE('',#19949,#4212);
#3225=LINE('',#19955,#4213);
#3226=LINE('',#19961,#4214);
#3227=LINE('',#19986,#4215);
#3228=LINE('',#19991,#4216);
#3229=LINE('',#19996,#4217);
#3230=LINE('',#20001,#4218);
#3231=LINE('',#20007,#4219);
#3232=LINE('',#20010,#4220);
#3233=LINE('',#20015,#4221);
#3234=LINE('',#20016,#4222);
#3235=LINE('',#20021,#4223);
#3236=LINE('',#20022,#4224);
#3237=LINE('',#20024,#4225);
#3238=LINE('',#20025,#4226);
#3239=LINE('',#20032,#4227);
#3240=LINE('',#20054,#4228);
#3241=LINE('',#20057,#4229);
#3242=LINE('',#20060,#4230);
#3243=LINE('',#20064,#4231);
#3244=LINE('',#20069,#4232);
#3245=LINE('',#20071,#4233);
#3246=LINE('',#20073,#4234);
#3247=LINE('',#20075,#4235);
#3248=LINE('',#20077,#4236);
#3249=LINE('',#20078,#4237);
#3250=LINE('',#20082,#4238);
#3251=LINE('',#20083,#4239);
#3252=LINE('',#20085,#4240);
#3253=LINE('',#20086,#4241);
#3254=LINE('',#20088,#4242);
#3255=LINE('',#20090,#4243);
#3256=LINE('',#20091,#4244);
#3257=LINE('',#20093,#4245);
#3258=LINE('',#20095,#4246);
#3259=LINE('',#20096,#4247);
#3260=LINE('',#20098,#4248);
#3261=LINE('',#20100,#4249);
#3262=LINE('',#20101,#4250);
#3263=LINE('',#20103,#4251);
#3264=LINE('',#20105,#4252);
#3265=LINE('',#20106,#4253);
#3266=LINE('',#20108,#4254);
#3267=LINE('',#20109,#4255);
#3268=VECTOR('',#12222,1.25);
#3269=VECTOR('',#12229,1.25);
#3270=VECTOR('',#12236,1.25);
#3271=VECTOR('',#12243,1.25);
#3272=VECTOR('',#12250,1.25);
#3273=VECTOR('',#12257,1.25);
#3274=VECTOR('',#12264,1.25);
#3275=VECTOR('',#12271,1.25);
#3276=VECTOR('',#12278,1.25);
#3277=VECTOR('',#12285,1.25);
#3278=VECTOR('',#12292,1.25);
#3279=VECTOR('',#12299,1.25);
#3280=VECTOR('',#12306,1.25);
#3281=VECTOR('',#12313,1.25);
#3282=VECTOR('',#12320,1.25);
#3283=VECTOR('',#12327,1.25);
#3284=VECTOR('',#12334,5.);
#3285=VECTOR('',#12339,1000.);
#3286=VECTOR('',#12342,1000.);
#3287=VECTOR('',#12347,1000.);
#3288=VECTOR('',#12348,1000.);
#3289=VECTOR('',#12349,1000.);
#3290=VECTOR('',#12352,1000.);
#3291=VECTOR('',#12355,1000.);
#3292=VECTOR('',#12360,1000.);
#3293=VECTOR('',#12361,1000.);
#3294=VECTOR('',#12362,1000.);
#3295=VECTOR('',#12365,1000.);
#3296=VECTOR('',#12372,1000.);
#3297=VECTOR('',#12373,1000.);
#3298=VECTOR('',#12374,1000.);
#3299=VECTOR('',#12377,1000.);
#3300=VECTOR('',#12380,1000.);
#3301=VECTOR('',#12385,1000.);
#3302=VECTOR('',#12386,1000.);
#3303=VECTOR('',#12389,1000.);
#3304=VECTOR('',#12392,1000.);
#3305=VECTOR('',#12393,1000.);
#3306=VECTOR('',#12396,1000.);
#3307=VECTOR('',#12399,1000.);
#3308=VECTOR('',#12404,1000.);
#3309=VECTOR('',#12405,1000.);
#3310=VECTOR('',#12406,1000.);
#3311=VECTOR('',#12411,1000.);
#3312=VECTOR('',#12416,1000.);
#3313=VECTOR('',#12419,1000.);
#3314=VECTOR('',#12420,1000.);
#3315=VECTOR('',#12423,1000.);
#3316=VECTOR('',#12426,1000.);
#3317=VECTOR('',#12429,1000.);
#3318=VECTOR('',#12434,1000.);
#3319=VECTOR('',#12437,1000.);
#3320=VECTOR('',#12440,1000.);
#3321=VECTOR('',#12443,1000.);
#3322=VECTOR('',#12446,1000.);
#3323=VECTOR('',#12447,1000.);
#3324=VECTOR('',#12448,1000.);
#3325=VECTOR('',#12451,1000.);
#3326=VECTOR('',#12454,1000.);
#3327=VECTOR('',#12455,1000.);
#3328=VECTOR('',#12458,1000.);
#3329=VECTOR('',#12465,1000.);
#3330=VECTOR('',#12468,1000.);
#3331=VECTOR('',#12473,1000.);
#3332=VECTOR('',#12476,1000.);
#3333=VECTOR('',#12479,1000.);
#3334=VECTOR('',#12480,1000.);
#3335=VECTOR('',#12483,1000.);
#3336=VECTOR('',#12484,1000.);
#3337=VECTOR('',#12487,1000.);
#3338=VECTOR('',#12488,1000.);
#3339=VECTOR('',#12491,1000.);
#3340=VECTOR('',#12492,1000.);
#3341=VECTOR('',#12515,5.5);
#3342=VECTOR('',#12522,14.);
#3343=VECTOR('',#12529,1.35);
#3344=VECTOR('',#12536,1.35);
#3345=VECTOR('',#12543,1.35);
#3346=VECTOR('',#12550,1.35);
#3347=VECTOR('',#12557,1.35);
#3348=VECTOR('',#12564,1.35);
#3349=VECTOR('',#12571,1.35);
#3350=VECTOR('',#12578,1.35);
#3351=VECTOR('',#12585,1.35);
#3352=VECTOR('',#12592,1.35);
#3353=VECTOR('',#12599,1.35);
#3354=VECTOR('',#12606,1.35);
#3355=VECTOR('',#12613,5.);
#3356=VECTOR('',#12620,7.5);
#3357=VECTOR('',#12627,2.75);
#3358=VECTOR('',#12634,5.);
#3359=VECTOR('',#12641,7.25);
#3360=VECTOR('',#12648,14.);
#3361=VECTOR('',#12655,4.75);
#3362=VECTOR('',#12662,2.75);
#3363=VECTOR('',#12667,1000.);
#3364=VECTOR('',#12668,1000.);
#3365=VECTOR('',#12669,1000.);
#3366=VECTOR('',#12670,1000.);
#3367=VECTOR('',#12675,1000.);
#3368=VECTOR('',#12680,1000.);
#3369=VECTOR('',#12687,1000.);
#3370=VECTOR('',#12696,1000.);
#3371=VECTOR('',#12703,1000.);
#3372=VECTOR('',#12704,1000.);
#3373=VECTOR('',#12705,1000.);
#3374=VECTOR('',#12706,1000.);
#3375=VECTOR('',#12707,1000.);
#3376=VECTOR('',#12708,1000.);
#3377=VECTOR('',#12709,1000.);
#3378=VECTOR('',#12710,1000.);
#3379=VECTOR('',#12711,1000.);
#3380=VECTOR('',#12712,1000.);
#3381=VECTOR('',#12713,1000.);
#3382=VECTOR('',#12714,1000.);
#3383=VECTOR('',#12715,1000.);
#3384=VECTOR('',#12716,1000.);
#3385=VECTOR('',#12717,1000.);
#3386=VECTOR('',#12718,1000.);
#3387=VECTOR('',#12719,1000.);
#3388=VECTOR('',#12730,1000.);
#3389=VECTOR('',#12731,1000.);
#3390=VECTOR('',#12732,1000.);
#3391=VECTOR('',#12737,1000.);
#3392=VECTOR('',#12738,1000.);
#3393=VECTOR('',#12739,1000.);
#3394=VECTOR('',#12744,1000.);
#3395=VECTOR('',#12745,1000.);
#3396=VECTOR('',#12746,1000.);
#3397=VECTOR('',#12749,1000.);
#3398=VECTOR('',#12756,1000.);
#3399=VECTOR('',#12763,1000.);
#3400=VECTOR('',#12770,1000.);
#3401=VECTOR('',#12773,1000.);
#3402=VECTOR('',#12776,1000.);
#3403=VECTOR('',#12779,1000.);
#3404=VECTOR('',#12782,1000.);
#3405=VECTOR('',#12785,1000.);
#3406=VECTOR('',#12788,1000.);
#3407=VECTOR('',#12791,1000.);
#3408=VECTOR('',#12794,1000.);
#3409=VECTOR('',#12797,1000.);
#3410=VECTOR('',#12800,1000.);
#3411=VECTOR('',#12803,1000.);
#3412=VECTOR('',#12806,1000.);
#3413=VECTOR('',#12809,1000.);
#3414=VECTOR('',#12812,1000.);
#3415=VECTOR('',#12815,1000.);
#3416=VECTOR('',#12818,1000.);
#3417=VECTOR('',#12823,1000.);
#3418=VECTOR('',#12832,1000.);
#3419=VECTOR('',#12837,1000.);
#3420=VECTOR('',#12842,1000.);
#3421=VECTOR('',#12849,1000.);
#3422=VECTOR('',#12864,1000.);
#3423=VECTOR('',#12867,1000.);
#3424=VECTOR('',#12872,1000.);
#3425=VECTOR('',#12875,1000.);
#3426=VECTOR('',#12878,1000.);
#3427=VECTOR('',#12881,1000.);
#3428=VECTOR('',#12884,1000.);
#3429=VECTOR('',#12897,1000.);
#3430=VECTOR('',#12898,1000.);
#3431=VECTOR('',#12899,1000.);
#3432=VECTOR('',#12900,1000.);
#3433=VECTOR('',#12901,1000.);
#3434=VECTOR('',#12902,1000.);
#3435=VECTOR('',#12905,1000.);
#3436=VECTOR('',#12906,1000.);
#3437=VECTOR('',#12909,1000.);
#3438=VECTOR('',#12910,1000.);
#3439=VECTOR('',#12911,1000.);
#3440=VECTOR('',#12912,1000.);
#3441=VECTOR('',#12913,1000.);
#3442=VECTOR('',#12914,1000.);
#3443=VECTOR('',#12915,1000.);
#3444=VECTOR('',#12916,1000.);
#3445=VECTOR('',#12917,1000.);
#3446=VECTOR('',#12918,1000.);
#3447=VECTOR('',#12919,1000.);
#3448=VECTOR('',#12920,1000.);
#3449=VECTOR('',#12921,1000.);
#3450=VECTOR('',#12922,1000.);
#3451=VECTOR('',#12923,1000.);
#3452=VECTOR('',#12924,1000.);
#3453=VECTOR('',#12925,1000.);
#3454=VECTOR('',#12926,1000.);
#3455=VECTOR('',#12927,1000.);
#3456=VECTOR('',#12928,1000.);
#3457=VECTOR('',#12929,1000.);
#3458=VECTOR('',#12930,1000.);
#3459=VECTOR('',#12931,1000.);
#3460=VECTOR('',#12932,1000.);
#3461=VECTOR('',#12933,1000.);
#3462=VECTOR('',#12934,1000.);
#3463=VECTOR('',#12935,1000.);
#3464=VECTOR('',#12936,1000.);
#3465=VECTOR('',#12937,1000.);
#3466=VECTOR('',#12938,1000.);
#3467=VECTOR('',#12939,1000.);
#3468=VECTOR('',#12940,1000.);
#3469=VECTOR('',#12941,1000.);
#3470=VECTOR('',#12942,1000.);
#3471=VECTOR('',#12943,1000.);
#3472=VECTOR('',#12944,1000.);
#3473=VECTOR('',#12945,1000.);
#3474=VECTOR('',#12946,1000.);
#3475=VECTOR('',#12949,1000.);
#3476=VECTOR('',#12950,1000.);
#3477=VECTOR('',#12953,1000.);
#3478=VECTOR('',#12954,1000.);
#3479=VECTOR('',#12955,1000.);
#3480=VECTOR('',#12956,1000.);
#3481=VECTOR('',#12957,1000.);
#3482=VECTOR('',#12960,1000.);
#3483=VECTOR('',#12963,1000.);
#3484=VECTOR('',#12966,1000.);
#3485=VECTOR('',#12967,1000.);
#3486=VECTOR('',#12968,1000.);
#3487=VECTOR('',#12969,1000.);
#3488=VECTOR('',#12970,1000.);
#3489=VECTOR('',#12971,1000.);
#3490=VECTOR('',#12972,1000.);
#3491=VECTOR('',#12973,1000.);
#3492=VECTOR('',#12974,1000.);
#3493=VECTOR('',#12975,1000.);
#3494=VECTOR('',#12976,1000.);
#3495=VECTOR('',#12977,1000.);
#3496=VECTOR('',#12978,1000.);
#3497=VECTOR('',#12979,1000.);
#3498=VECTOR('',#12984,1000.);
#3499=VECTOR('',#12987,1000.);
#3500=VECTOR('',#12988,1000.);
#3501=VECTOR('',#12995,1000.);
#3502=VECTOR('',#13000,1000.);
#3503=VECTOR('',#13001,1000.);
#3504=VECTOR('',#13002,1000.);
#3505=VECTOR('',#13003,1000.);
#3506=VECTOR('',#13004,1000.);
#3507=VECTOR('',#13005,1000.);
#3508=VECTOR('',#13006,1000.);
#3509=VECTOR('',#13007,1000.);
#3510=VECTOR('',#13008,1000.);
#3511=VECTOR('',#13009,1000.);
#3512=VECTOR('',#13016,1000.);
#3513=VECTOR('',#13021,1000.);
#3514=VECTOR('',#13022,1000.);
#3515=VECTOR('',#13027,1000.);
#3516=VECTOR('',#13030,1000.);
#3517=VECTOR('',#13031,1000.);
#3518=VECTOR('',#13032,1000.);
#3519=VECTOR('',#13033,1000.);
#3520=VECTOR('',#13034,1000.);
#3521=VECTOR('',#13035,1000.);
#3522=VECTOR('',#13036,1000.);
#3523=VECTOR('',#13037,1000.);
#3524=VECTOR('',#13038,1000.);
#3525=VECTOR('',#13039,1000.);
#3526=VECTOR('',#13040,1000.);
#3527=VECTOR('',#13041,1000.);
#3528=VECTOR('',#13042,1000.);
#3529=VECTOR('',#13043,1000.);
#3530=VECTOR('',#13056,1000.);
#3531=VECTOR('',#13057,1000.);
#3532=VECTOR('',#13060,1000.);
#3533=VECTOR('',#13065,1000.);
#3534=VECTOR('',#13066,1000.);
#3535=VECTOR('',#13071,1000.);
#3536=VECTOR('',#13074,1000.);
#3537=VECTOR('',#13075,1000.);
#3538=VECTOR('',#13080,1000.);
#3539=VECTOR('',#13083,1000.);
#3540=VECTOR('',#13084,1000.);
#3541=VECTOR('',#13087,1000.);
#3542=VECTOR('',#13092,1000.);
#3543=VECTOR('',#13093,1000.);
#3544=VECTOR('',#13098,1000.);
#3545=VECTOR('',#13101,1000.);
#3546=VECTOR('',#13102,1000.);
#3547=VECTOR('',#13107,1000.);
#3548=VECTOR('',#13110,1000.);
#3549=VECTOR('',#13111,1000.);
#3550=VECTOR('',#13114,1000.);
#3551=VECTOR('',#13119,1000.);
#3552=VECTOR('',#13120,1000.);
#3553=VECTOR('',#13125,1000.);
#3554=VECTOR('',#13128,1000.);
#3555=VECTOR('',#13129,1000.);
#3556=VECTOR('',#13134,1000.);
#3557=VECTOR('',#13137,1000.);
#3558=VECTOR('',#13138,1000.);
#3559=VECTOR('',#13141,1000.);
#3560=VECTOR('',#13146,1000.);
#3561=VECTOR('',#13155,1000.);
#3562=VECTOR('',#13156,1000.);
#3563=VECTOR('',#13157,1000.);
#3564=VECTOR('',#13158,1000.);
#3565=VECTOR('',#13159,1000.);
#3566=VECTOR('',#13164,1000.);
#3567=VECTOR('',#13165,1000.);
#3568=VECTOR('',#13166,1000.);
#3569=VECTOR('',#13169,1000.);
#3570=VECTOR('',#13170,1000.);
#3571=VECTOR('',#13171,1000.);
#3572=VECTOR('',#13174,1000.);
#3573=VECTOR('',#13175,1000.);
#3574=VECTOR('',#13176,1000.);
#3575=VECTOR('',#13179,1000.);
#3576=VECTOR('',#13180,1000.);
#3577=VECTOR('',#13183,1000.);
#3578=VECTOR('',#13184,1000.);
#3579=VECTOR('',#13187,1000.);
#3580=VECTOR('',#13188,1000.);
#3581=VECTOR('',#13189,1000.);
#3582=VECTOR('',#13192,1000.);
#3583=VECTOR('',#13193,1000.);
#3584=VECTOR('',#13194,1000.);
#3585=VECTOR('',#13195,1000.);
#3586=VECTOR('',#13196,1000.);
#3587=VECTOR('',#13197,1000.);
#3588=VECTOR('',#13198,1000.);
#3589=VECTOR('',#13199,1000.);
#3590=VECTOR('',#13200,1000.);
#3591=VECTOR('',#13201,1000.);
#3592=VECTOR('',#13202,1000.);
#3593=VECTOR('',#13203,1000.);
#3594=VECTOR('',#13204,1000.);
#3595=VECTOR('',#13205,1000.);
#3596=VECTOR('',#13206,1000.);
#3597=VECTOR('',#13207,1000.);
#3598=VECTOR('',#13208,1000.);
#3599=VECTOR('',#13209,1000.);
#3600=VECTOR('',#13210,1000.);
#3601=VECTOR('',#13211,1000.);
#3602=VECTOR('',#13212,1000.);
#3603=VECTOR('',#13213,1000.);
#3604=VECTOR('',#13214,1000.);
#3605=VECTOR('',#13215,1000.);
#3606=VECTOR('',#13216,1000.);
#3607=VECTOR('',#13217,1000.);
#3608=VECTOR('',#13218,1000.);
#3609=VECTOR('',#13219,1000.);
#3610=VECTOR('',#13220,1000.);
#3611=VECTOR('',#13221,1000.);
#3612=VECTOR('',#13222,1000.);
#3613=VECTOR('',#13223,1000.);
#3614=VECTOR('',#13224,1000.);
#3615=VECTOR('',#13225,1000.);
#3616=VECTOR('',#13226,1000.);
#3617=VECTOR('',#13227,1000.);
#3618=VECTOR('',#13228,1000.);
#3619=VECTOR('',#13231,1000.);
#3620=VECTOR('',#13232,1000.);
#3621=VECTOR('',#13233,1000.);
#3622=VECTOR('',#13234,1000.);
#3623=VECTOR('',#13235,1000.);
#3624=VECTOR('',#13238,1000.);
#3625=VECTOR('',#13239,1000.);
#3626=VECTOR('',#13240,1000.);
#3627=VECTOR('',#13241,1000.);
#3628=VECTOR('',#13242,1000.);
#3629=VECTOR('',#13243,1000.);
#3630=VECTOR('',#13244,1000.);
#3631=VECTOR('',#13245,1000.);
#3632=VECTOR('',#13246,1000.);
#3633=VECTOR('',#13247,1000.);
#3634=VECTOR('',#13248,1000.);
#3635=VECTOR('',#13249,1000.);
#3636=VECTOR('',#13250,1000.);
#3637=VECTOR('',#13251,1000.);
#3638=VECTOR('',#13252,1000.);
#3639=VECTOR('',#13255,1000.);
#3640=VECTOR('',#13260,1000.);
#3641=VECTOR('',#13261,1000.);
#3642=VECTOR('',#13264,1000.);
#3643=VECTOR('',#13273,1000.);
#3644=VECTOR('',#13274,1000.);
#3645=VECTOR('',#13275,1000.);
#3646=VECTOR('',#13276,1000.);
#3647=VECTOR('',#13277,1000.);
#3648=VECTOR('',#13278,1000.);
#3649=VECTOR('',#13279,1000.);
#3650=VECTOR('',#13280,1000.);
#3651=VECTOR('',#13281,1000.);
#3652=VECTOR('',#13282,1000.);
#3653=VECTOR('',#13285,1000.);
#3654=VECTOR('',#13294,1000.);
#3655=VECTOR('',#13295,1000.);
#3656=VECTOR('',#13298,1000.);
#3657=VECTOR('',#13303,1000.);
#3658=VECTOR('',#13304,1000.);
#3659=VECTOR('',#13305,1000.);
#3660=VECTOR('',#13306,1000.);
#3661=VECTOR('',#13307,1000.);
#3662=VECTOR('',#13308,1000.);
#3663=VECTOR('',#13309,1000.);
#3664=VECTOR('',#13310,1000.);
#3665=VECTOR('',#13311,1000.);
#3666=VECTOR('',#13312,1000.);
#3667=VECTOR('',#13313,1000.);
#3668=VECTOR('',#13314,1000.);
#3669=VECTOR('',#13315,1000.);
#3670=VECTOR('',#13316,1000.);
#3671=VECTOR('',#13327,1000.);
#3672=VECTOR('',#13328,1000.);
#3673=VECTOR('',#13329,1000.);
#3674=VECTOR('',#13332,1000.);
#3675=VECTOR('',#13333,1000.);
#3676=VECTOR('',#13338,1000.);
#3677=VECTOR('',#13339,1000.);
#3678=VECTOR('',#13340,1000.);
#3679=VECTOR('',#13343,1000.);
#3680=VECTOR('',#13344,1000.);
#3681=VECTOR('',#13347,1000.);
#3682=VECTOR('',#13350,1000.);
#3683=VECTOR('',#13355,1000.);
#3684=VECTOR('',#13356,1000.);
#3685=VECTOR('',#13357,1000.);
#3686=VECTOR('',#13358,1000.);
#3687=VECTOR('',#13361,1000.);
#3688=VECTOR('',#13362,1000.);
#3689=VECTOR('',#13367,1000.);
#3690=VECTOR('',#13368,1000.);
#3691=VECTOR('',#13369,1000.);
#3692=VECTOR('',#13372,1000.);
#3693=VECTOR('',#13373,1000.);
#3694=VECTOR('',#13376,1000.);
#3695=VECTOR('',#13377,1000.);
#3696=VECTOR('',#13378,1000.);
#3697=VECTOR('',#13381,1000.);
#3698=VECTOR('',#13382,1000.);
#3699=VECTOR('',#13385,1000.);
#3700=VECTOR('',#13386,1000.);
#3701=VECTOR('',#13389,1000.);
#3702=VECTOR('',#13390,1000.);
#3703=VECTOR('',#13391,1000.);
#3704=VECTOR('',#13394,1000.);
#3705=VECTOR('',#13395,1000.);
#3706=VECTOR('',#13396,1000.);
#3707=VECTOR('',#13397,1000.);
#3708=VECTOR('',#13400,1000.);
#3709=VECTOR('',#13401,1000.);
#3710=VECTOR('',#13404,1000.);
#3711=VECTOR('',#13405,1000.);
#3712=VECTOR('',#13406,1000.);
#3713=VECTOR('',#13409,1000.);
#3714=VECTOR('',#13412,1000.);
#3715=VECTOR('',#13415,1000.);
#3716=VECTOR('',#13418,1000.);
#3717=VECTOR('',#13419,1000.);
#3718=VECTOR('',#13422,1000.);
#3719=VECTOR('',#13423,1000.);
#3720=VECTOR('',#13426,1000.);
#3721=VECTOR('',#13427,1000.);
#3722=VECTOR('',#13428,1000.);
#3723=VECTOR('',#13433,1000.);
#3724=VECTOR('',#13434,1000.);
#3725=VECTOR('',#13437,1000.);
#3726=VECTOR('',#13438,1000.);
#3727=VECTOR('',#13439,1000.);
#3728=VECTOR('',#13442,1000.);
#3729=VECTOR('',#13445,1000.);
#3730=VECTOR('',#13448,1000.);
#3731=VECTOR('',#13451,1000.);
#3732=VECTOR('',#13452,1000.);
#3733=VECTOR('',#13455,1000.);
#3734=VECTOR('',#13456,1000.);
#3735=VECTOR('',#13459,1000.);
#3736=VECTOR('',#13460,1000.);
#3737=VECTOR('',#13461,1000.);
#3738=VECTOR('',#13464,1000.);
#3739=VECTOR('',#13471,1000.);
#3740=VECTOR('',#13472,1000.);
#3741=VECTOR('',#13475,1000.);
#3742=VECTOR('',#13476,1000.);
#3743=VECTOR('',#13477,1000.);
#3744=VECTOR('',#13478,1000.);
#3745=VECTOR('',#13481,1000.);
#3746=VECTOR('',#13482,1000.);
#3747=VECTOR('',#13483,1000.);
#3748=VECTOR('',#13484,1000.);
#3749=VECTOR('',#13487,1000.);
#3750=VECTOR('',#13488,1000.);
#3751=VECTOR('',#13489,1000.);
#3752=VECTOR('',#13490,1000.);
#3753=VECTOR('',#13493,1000.);
#3754=VECTOR('',#13494,1000.);
#3755=VECTOR('',#13495,1000.);
#3756=VECTOR('',#13496,1000.);
#3757=VECTOR('',#13499,1000.);
#3758=VECTOR('',#13500,1000.);
#3759=VECTOR('',#13501,1000.);
#3760=VECTOR('',#13502,1000.);
#3761=VECTOR('',#13505,1000.);
#3762=VECTOR('',#13506,1000.);
#3763=VECTOR('',#13507,1000.);
#3764=VECTOR('',#13510,1000.);
#3765=VECTOR('',#13511,1000.);
#3766=VECTOR('',#13514,1000.);
#3767=VECTOR('',#13515,1000.);
#3768=VECTOR('',#13518,1000.);
#3769=VECTOR('',#13521,1000.);
#3770=VECTOR('',#13524,1000.);
#3771=VECTOR('',#13525,1000.);
#3772=VECTOR('',#13528,1000.);
#3773=VECTOR('',#13529,1000.);
#3774=VECTOR('',#13532,1000.);
#3775=VECTOR('',#13533,1000.);
#3776=VECTOR('',#13534,1000.);
#3777=VECTOR('',#13537,1000.);
#3778=VECTOR('',#13538,1000.);
#3779=VECTOR('',#13541,1000.);
#3780=VECTOR('',#13544,1000.);
#3781=VECTOR('',#13545,1000.);
#3782=VECTOR('',#13548,1000.);
#3783=VECTOR('',#13549,1000.);
#3784=VECTOR('',#13550,1000.);
#3785=VECTOR('',#13553,1000.);
#3786=VECTOR('',#13554,1000.);
#3787=VECTOR('',#13557,1000.);
#3788=VECTOR('',#13558,1000.);
#3789=VECTOR('',#13561,1000.);
#3790=VECTOR('',#13562,1000.);
#3791=VECTOR('',#13565,1000.);
#3792=VECTOR('',#13568,1000.);
#3793=VECTOR('',#13571,1000.);
#3794=VECTOR('',#13574,1000.);
#3795=VECTOR('',#13647,1000.);
#3796=VECTOR('',#13650,1000.);
#3797=VECTOR('',#13651,1000.);
#3798=VECTOR('',#13654,1000.);
#3799=VECTOR('',#13657,1000.);
#3800=VECTOR('',#13660,1000.);
#3801=VECTOR('',#13663,1000.);
#3802=VECTOR('',#13666,1000.);
#3803=VECTOR('',#13667,1000.);
#3804=VECTOR('',#13670,1000.);
#3805=VECTOR('',#13671,1000.);
#3806=VECTOR('',#13674,1000.);
#3807=VECTOR('',#13675,1000.);
#3808=VECTOR('',#13676,1000.);
#3809=VECTOR('',#13679,1000.);
#3810=VECTOR('',#13682,1000.);
#3811=VECTOR('',#13685,1000.);
#3812=VECTOR('',#13688,1000.);
#3813=VECTOR('',#13689,1000.);
#3814=VECTOR('',#13692,1000.);
#3815=VECTOR('',#13693,1000.);
#3816=VECTOR('',#13696,1000.);
#3817=VECTOR('',#13697,1000.);
#3818=VECTOR('',#13700,1000.);
#3819=VECTOR('',#13701,1000.);
#3820=VECTOR('',#13704,1000.);
#3821=VECTOR('',#13707,1000.);
#3822=VECTOR('',#13710,1000.);
#3823=VECTOR('',#13711,1000.);
#3824=VECTOR('',#13714,1000.);
#3825=VECTOR('',#13715,1000.);
#3826=VECTOR('',#13716,1000.);
#3827=VECTOR('',#13719,1000.);
#3828=VECTOR('',#13720,1000.);
#3829=VECTOR('',#13723,1000.);
#3830=VECTOR('',#13724,1000.);
#3831=VECTOR('',#13725,1000.);
#3832=VECTOR('',#13728,1000.);
#3833=VECTOR('',#13729,1000.);
#3834=VECTOR('',#13732,1000.);
#3835=VECTOR('',#13733,1000.);
#3836=VECTOR('',#13736,1000.);
#3837=VECTOR('',#13737,1000.);
#3838=VECTOR('',#13740,1000.);
#3839=VECTOR('',#13741,1000.);
#3840=VECTOR('',#13746,1000.);
#3841=VECTOR('',#13747,1000.);
#3842=VECTOR('',#13748,1000.);
#3843=VECTOR('',#13753,1000.);
#3844=VECTOR('',#13756,1000.);
#3845=VECTOR('',#13757,1000.);
#3846=VECTOR('',#13758,1000.);
#3847=VECTOR('',#13759,1000.);
#3848=VECTOR('',#13762,1000.);
#3849=VECTOR('',#13763,1000.);
#3850=VECTOR('',#13768,1000.);
#3851=VECTOR('',#13769,1000.);
#3852=VECTOR('',#13772,1000.);
#3853=VECTOR('',#13773,1000.);
#3854=VECTOR('',#13774,1000.);
#3855=VECTOR('',#13775,1000.);
#3856=VECTOR('',#13778,1000.);
#3857=VECTOR('',#13779,1000.);
#3858=VECTOR('',#13780,1000.);
#3859=VECTOR('',#13781,1000.);
#3860=VECTOR('',#13784,1000.);
#3861=VECTOR('',#13785,1000.);
#3862=VECTOR('',#13786,1000.);
#3863=VECTOR('',#13789,1000.);
#3864=VECTOR('',#13790,1000.);
#3865=VECTOR('',#13791,1000.);
#3866=VECTOR('',#13792,1000.);
#3867=VECTOR('',#13795,1000.);
#3868=VECTOR('',#13796,1000.);
#3869=VECTOR('',#13797,1000.);
#3870=VECTOR('',#13798,1000.);
#3871=VECTOR('',#13801,1000.);
#3872=VECTOR('',#13802,1000.);
#3873=VECTOR('',#13803,1000.);
#3874=VECTOR('',#13806,1000.);
#3875=VECTOR('',#13809,1000.);
#3876=VECTOR('',#13812,1000.);
#3877=VECTOR('',#13815,1000.);
#3878=VECTOR('',#13816,1000.);
#3879=VECTOR('',#13819,1000.);
#3880=VECTOR('',#13820,1000.);
#3881=VECTOR('',#13821,1000.);
#3882=VECTOR('',#13824,1000.);
#3883=VECTOR('',#13825,1000.);
#3884=VECTOR('',#13828,1000.);
#3885=VECTOR('',#13829,1000.);
#3886=VECTOR('',#13832,1000.);
#3887=VECTOR('',#13833,1000.);
#3888=VECTOR('',#13836,1000.);
#3889=VECTOR('',#13839,1000.);
#3890=VECTOR('',#13842,1000.);
#3891=VECTOR('',#13847,1000.);
#3892=VECTOR('',#13850,1000.);
#3893=VECTOR('',#13853,1000.);
#3894=VECTOR('',#13854,1000.);
#3895=VECTOR('',#13857,1000.);
#3896=VECTOR('',#13858,1000.);
#3897=VECTOR('',#13859,1000.);
#3898=VECTOR('',#13860,1000.);
#3899=VECTOR('',#13861,1000.);
#3900=VECTOR('',#13862,1000.);
#3901=VECTOR('',#13863,1000.);
#3902=VECTOR('',#13864,1000.);
#3903=VECTOR('',#13867,1000.);
#3904=VECTOR('',#13868,1000.);
#3905=VECTOR('',#13869,1000.);
#3906=VECTOR('',#13874,1000.);
#3907=VECTOR('',#13877,1000.);
#3908=VECTOR('',#13878,1000.);
#3909=VECTOR('',#13879,1000.);
#3910=VECTOR('',#13880,1000.);
#3911=VECTOR('',#13881,1000.);
#3912=VECTOR('',#13886,1000.);
#3913=VECTOR('',#13891,1000.);
#3914=VECTOR('',#13898,1000.);
#3915=VECTOR('',#13903,1000.);
#3916=VECTOR('',#13906,1000.);
#3917=VECTOR('',#13907,1000.);
#3918=VECTOR('',#13910,1000.);
#3919=VECTOR('',#13911,1000.);
#3920=VECTOR('',#13914,1000.);
#3921=VECTOR('',#13919,1000.);
#3922=VECTOR('',#13924,1000.);
#3923=VECTOR('',#13925,1000.);
#3924=VECTOR('',#13928,1000.);
#3925=VECTOR('',#13949,1000.);
#3926=VECTOR('',#13954,1000.);
#3927=VECTOR('',#13959,1000.);
#3928=VECTOR('',#13960,1000.);
#3929=VECTOR('',#13961,1000.);
#3930=VECTOR('',#13962,1000.);
#3931=VECTOR('',#13963,1000.);
#3932=VECTOR('',#13968,1000.);
#3933=VECTOR('',#13971,1000.);
#3934=VECTOR('',#13972,1000.);
#3935=VECTOR('',#13975,1000.);
#3936=VECTOR('',#13976,1000.);
#3937=VECTOR('',#13979,1000.);
#3938=VECTOR('',#13980,1000.);
#3939=VECTOR('',#13995,1000.);
#3940=VECTOR('',#13996,1000.);
#3941=VECTOR('',#13997,1000.);
#3942=VECTOR('',#14000,1000.);
#3943=VECTOR('',#14001,1000.);
#3944=VECTOR('',#14004,1000.);
#3945=VECTOR('',#14005,1000.);
#3946=VECTOR('',#14008,1000.);
#3947=VECTOR('',#14011,1000.);
#3948=VECTOR('',#14012,1000.);
#3949=VECTOR('',#14013,1000.);
#3950=VECTOR('',#14016,1000.);
#3951=VECTOR('',#14017,1000.);
#3952=VECTOR('',#14020,1000.);
#3953=VECTOR('',#14021,1000.);
#3954=VECTOR('',#14024,1000.);
#3955=VECTOR('',#14047,1.25);
#3956=VECTOR('',#14054,1.25);
#3957=VECTOR('',#14061,1.25);
#3958=VECTOR('',#14068,1.25);
#3959=VECTOR('',#14075,1.025);
#3960=VECTOR('',#14082,1.025);
#3961=VECTOR('',#14089,1.025);
#3962=VECTOR('',#14096,1.025);
#3963=VECTOR('',#14103,1.25);
#3964=VECTOR('',#14110,1.25);
#3965=VECTOR('',#14117,1.25);
#3966=VECTOR('',#14124,1.25);
#3967=VECTOR('',#14131,1.025);
#3968=VECTOR('',#14138,1.025);
#3969=VECTOR('',#14145,1.025);
#3970=VECTOR('',#14152,1.025);
#3971=VECTOR('',#14159,1.25);
#3972=VECTOR('',#14166,1.25);
#3973=VECTOR('',#14173,1.25);
#3974=VECTOR('',#14180,1.25);
#3975=VECTOR('',#14187,1.25);
#3976=VECTOR('',#14194,1.25);
#3977=VECTOR('',#14201,1.25);
#3978=VECTOR('',#14208,1.25);
#3979=VECTOR('',#14215,5.);
#3980=VECTOR('',#14220,1.34999999991669);
#3981=VECTOR('',#14225,1.34999999991669);
#3982=VECTOR('',#14230,1.34999999991669);
#3983=VECTOR('',#14235,1.34999999991669);
#3984=VECTOR('',#14240,1.34999999990714);
#3985=VECTOR('',#14245,1.34999999990714);
#3986=VECTOR('',#14250,1.34999999990714);
#3987=VECTOR('',#14255,1.34999999990714);
#3988=VECTOR('',#14260,5.19997115839037);
#3989=VECTOR('',#14267,1.3);
#3990=VECTOR('',#14274,1.3);
#3991=VECTOR('',#14281,1.3);
#3992=VECTOR('',#14288,1.3);
#3993=VECTOR('',#14295,1.3);
#3994=VECTOR('',#14302,1.3);
#3995=VECTOR('',#14309,1.3);
#3996=VECTOR('',#14316,1.3);
#3997=VECTOR('',#14321,1000.);
#3998=VECTOR('',#14322,1000.);
#3999=VECTOR('',#14325,1000.);
#4000=VECTOR('',#14328,1000.);
#4001=VECTOR('',#14335,1000.);
#4002=VECTOR('',#14338,1000.);
#4003=VECTOR('',#14339,1000.);
#4004=VECTOR('',#14340,1000.);
#4005=VECTOR('',#14343,1000.);
#4006=VECTOR('',#14346,1000.);
#4007=VECTOR('',#14347,1000.);
#4008=VECTOR('',#14348,1000.);
#4009=VECTOR('',#14353,1000.);
#4010=VECTOR('',#14358,1000.);
#4011=VECTOR('',#14359,1000.);
#4012=VECTOR('',#14362,1000.);
#4013=VECTOR('',#14365,1000.);
#4014=VECTOR('',#14366,1000.);
#4015=VECTOR('',#14371,1000.);
#4016=VECTOR('',#14372,1000.);
#4017=VECTOR('',#14375,1000.);
#4018=VECTOR('',#14376,1000.);
#4019=VECTOR('',#14379,1000.);
#4020=VECTOR('',#14382,1000.);
#4021=VECTOR('',#14385,1000.);
#4022=VECTOR('',#14388,1000.);
#4023=VECTOR('',#14389,1000.);
#4024=VECTOR('',#14394,1000.);
#4025=VECTOR('',#14397,1000.);
#4026=VECTOR('',#14400,1000.);
#4027=VECTOR('',#14403,1000.);
#4028=VECTOR('',#14410,1000.);
#4029=VECTOR('',#14413,1000.);
#4030=VECTOR('',#14414,1000.);
#4031=VECTOR('',#14415,1000.);
#4032=VECTOR('',#14416,1000.);
#4033=VECTOR('',#14421,1000.);
#4034=VECTOR('',#14424,1000.);
#4035=VECTOR('',#14427,1000.);
#4036=VECTOR('',#14430,1000.);
#4037=VECTOR('',#14431,1000.);
#4038=VECTOR('',#14436,1000.);
#4039=VECTOR('',#14437,1000.);
#4040=VECTOR('',#14440,1000.);
#4041=VECTOR('',#14441,1000.);
#4042=VECTOR('',#14442,1000.);
#4043=VECTOR('',#14447,1000.);
#4044=VECTOR('',#14450,1000.);
#4045=VECTOR('',#14453,1000.);
#4046=VECTOR('',#14456,1000.);
#4047=VECTOR('',#14463,1000.);
#4048=VECTOR('',#14466,1000.);
#4049=VECTOR('',#14475,1.25);
#4050=VECTOR('',#14482,1.25);
#4051=VECTOR('',#14489,1.25);
#4052=VECTOR('',#14496,1.25);
#4053=VECTOR('',#14503,1.25);
#4054=VECTOR('',#14510,1.25);
#4055=VECTOR('',#14517,1.25);
#4056=VECTOR('',#14524,1.25);
#4057=VECTOR('',#14533,4.59);
#4058=VECTOR('',#14542,1.25);
#4059=VECTOR('',#14549,1.25);
#4060=VECTOR('',#14556,1.25);
#4061=VECTOR('',#14563,1.25);
#4062=VECTOR('',#14570,1.25);
#4063=VECTOR('',#14577,1.25);
#4064=VECTOR('',#14584,1.25);
#4065=VECTOR('',#14591,1.25);
#4066=VECTOR('',#14598,5.5);
#4067=VECTOR('',#14603,2.5);
#4068=VECTOR('',#14608,1000.);
#4069=VECTOR('',#14611,1000.);
#4070=VECTOR('',#14618,1000.);
#4071=VECTOR('',#14621,1000.);
#4072=VECTOR('',#14624,1000.);
#4073=VECTOR('',#14625,1000.);
#4074=VECTOR('',#14628,1000.);
#4075=VECTOR('',#14629,1000.);
#4076=VECTOR('',#14642,12.5);
#4077=VECTOR('',#14649,12.5);
#4078=VECTOR('',#14656,12.5);
#4079=VECTOR('',#14663,1000.);
#4080=VECTOR('',#14666,1000.);
#4081=VECTOR('',#14671,8.);
#4082=VECTOR('',#14678,8.);
#4083=VECTOR('',#14683,1000.);
#4084=VECTOR('',#14684,1000.);
#4085=VECTOR('',#14685,1000.);
#4086=VECTOR('',#14686,1000.);
#4087=VECTOR('',#14687,1000.);
#4088=VECTOR('',#14688,1000.);
#4089=VECTOR('',#14689,1000.);
#4090=VECTOR('',#14690,1000.);
#4091=VECTOR('',#14691,1000.);
#4092=VECTOR('',#14692,1000.);
#4093=VECTOR('',#14695,1000.);
#4094=VECTOR('',#14696,1000.);
#4095=VECTOR('',#14697,1000.);
#4096=VECTOR('',#14700,1000.);
#4097=VECTOR('',#14701,1000.);
#4098=VECTOR('',#14702,1000.);
#4099=VECTOR('',#14705,1000.);
#4100=VECTOR('',#14706,1000.);
#4101=VECTOR('',#14707,1000.);
#4102=VECTOR('',#14708,1000.);
#4103=VECTOR('',#14711,1000.);
#4104=VECTOR('',#14712,1000.);
#4105=VECTOR('',#14713,1000.);
#4106=VECTOR('',#14716,1000.);
#4107=VECTOR('',#14717,1000.);
#4108=VECTOR('',#14718,1000.);
#4109=VECTOR('',#14719,1000.);
#4110=VECTOR('',#14720,1000.);
#4111=VECTOR('',#14721,1000.);
#4112=VECTOR('',#14722,1000.);
#4113=VECTOR('',#14725,1000.);
#4114=VECTOR('',#14726,1000.);
#4115=VECTOR('',#14727,1000.);
#4116=VECTOR('',#14728,1000.);
#4117=VECTOR('',#14743,1000.);
#4118=VECTOR('',#14746,1000.);
#4119=VECTOR('',#14751,1000.);
#4120=VECTOR('',#14756,1000.);
#4121=VECTOR('',#14767,1000.);
#4122=VECTOR('',#14776,1000.);
#4123=VECTOR('',#14777,1000.);
#4124=VECTOR('',#14778,1000.);
#4125=VECTOR('',#14779,1000.);
#4126=VECTOR('',#14782,1000.);
#4127=VECTOR('',#14783,1000.);
#4128=VECTOR('',#14784,1000.);
#4129=VECTOR('',#14787,1000.);
#4130=VECTOR('',#14788,1000.);
#4131=VECTOR('',#14789,1000.);
#4132=VECTOR('',#14792,1000.);
#4133=VECTOR('',#14793,1000.);
#4134=VECTOR('',#14806,8.);
#4135=VECTOR('',#14813,1.25);
#4136=VECTOR('',#14820,1.25);
#4137=VECTOR('',#14827,1.25);
#4138=VECTOR('',#14834,1.25);
#4139=VECTOR('',#14839,1000.);
#4140=VECTOR('',#14840,1000.);
#4141=VECTOR('',#14841,1000.);
#4142=VECTOR('',#14842,1000.);
#4143=VECTOR('',#14845,1000.);
#4144=VECTOR('',#14846,1000.);
#4145=VECTOR('',#14847,1000.);
#4146=VECTOR('',#14848,1000.);
#4147=VECTOR('',#14849,1000.);
#4148=VECTOR('',#14852,1000.);
#4149=VECTOR('',#14853,1000.);
#4150=VECTOR('',#14854,1000.);
#4151=VECTOR('',#14857,1000.);
#4152=VECTOR('',#14858,1000.);
#4153=VECTOR('',#14859,1000.);
#4154=VECTOR('',#14860,1000.);
#4155=VECTOR('',#14861,1000.);
#4156=VECTOR('',#14864,1000.);
#4157=VECTOR('',#14865,1000.);
#4158=VECTOR('',#14866,1000.);
#4159=VECTOR('',#14869,1000.);
#4160=VECTOR('',#14870,1000.);
#4161=VECTOR('',#14871,1000.);
#4162=VECTOR('',#14872,1000.);
#4163=VECTOR('',#14873,1000.);
#4164=VECTOR('',#14876,1000.);
#4165=VECTOR('',#14877,1000.);
#4166=VECTOR('',#14878,1000.);
#4167=VECTOR('',#14879,1000.);
#4168=VECTOR('',#14880,1000.);
#4169=VECTOR('',#14883,1000.);
#4170=VECTOR('',#14884,1000.);
#4171=VECTOR('',#14885,1000.);
#4172=VECTOR('',#14886,1000.);
#4173=VECTOR('',#14887,1000.);
#4174=VECTOR('',#14888,1000.);
#4175=VECTOR('',#14889,1000.);
#4176=VECTOR('',#14892,1000.);
#4177=VECTOR('',#14893,1000.);
#4178=VECTOR('',#14894,1000.);
#4179=VECTOR('',#14895,1000.);
#4180=VECTOR('',#14896,1000.);
#4181=VECTOR('',#14897,1000.);
#4182=VECTOR('',#14898,1000.);
#4183=VECTOR('',#14911,1000.);
#4184=VECTOR('',#14914,1000.);
#4185=VECTOR('',#14917,1000.);
#4186=VECTOR('',#14918,1000.);
#4187=VECTOR('',#14919,1000.);
#4188=VECTOR('',#14922,1000.);
#4189=VECTOR('',#14923,1000.);
#4190=VECTOR('',#14924,1000.);
#4191=VECTOR('',#14939,1000.);
#4192=VECTOR('',#14942,1000.);
#4193=VECTOR('',#14945,1000.);
#4194=VECTOR('',#14948,1000.);
#4195=VECTOR('',#14967,4.25);
#4196=VECTOR('',#14976,4.);
#4197=VECTOR('',#14979,4.);
#4198=VECTOR('',#14984,5.51648351648352);
#4199=VECTOR('',#14991,5.51648351648352);
#4200=VECTOR('',#15048,6.48351648351648);
#4201=VECTOR('',#15055,5.51648351648352);
#4202=VECTOR('',#15066,6.48351648351649);
#4203=VECTOR('',#15073,5.51648351648352);
#4204=VECTOR('',#15084,9.);
#4205=VECTOR('',#15091,6.48351648351648);
#4206=VECTOR('',#15104,6.48351648351648);
#4207=VECTOR('',#15111,8.);
#4208=VECTOR('',#15116,8.);
#4209=VECTOR('',#15131,5.);
#4210=VECTOR('',#15138,2.1);
#4211=VECTOR('',#15145,4.);
#4212=VECTOR('',#15160,5.);
#4213=VECTOR('',#15167,1.6);
#4214=VECTOR('',#15174,4.);
#4215=VECTOR('',#15219,4.59);
#4216=VECTOR('',#15226,2.24999999999999);
#4217=VECTOR('',#15231,4.59);
#4218=VECTOR('',#15238,2.24999999999999);
#4219=VECTOR('',#15243,1000.);
#4220=VECTOR('',#15246,1000.);
#4221=VECTOR('',#15251,1000.);
#4222=VECTOR('',#15252,1000.);
#4223=VECTOR('',#15257,1000.);
#4224=VECTOR('',#15258,1000.);
#4225=VECTOR('',#15261,1000.);
#4226=VECTOR('',#15262,1000.);
#4227=VECTOR('',#15271,1.25);
#4228=VECTOR('',#15296,3.9);
#4229=VECTOR('',#15301,3.9);
#4230=VECTOR('',#15304,2.);
#4231=VECTOR('',#15309,1.61);
#4232=VECTOR('',#15314,1000.);
#4233=VECTOR('',#15315,1000.);
#4234=VECTOR('',#15316,1000.);
#4235=VECTOR('',#15317,1000.);
#4236=VECTOR('',#15318,1000.);
#4237=VECTOR('',#15319,1000.);
#4238=VECTOR('',#15324,1000.);
#4239=VECTOR('',#15325,1000.);
#4240=VECTOR('',#15326,1000.);
#4241=VECTOR('',#15327,1000.);
#4242=VECTOR('',#15330,1000.);
#4243=VECTOR('',#15331,1000.);
#4244=VECTOR('',#15332,1000.);
#4245=VECTOR('',#15335,1000.);
#4246=VECTOR('',#15336,1000.);
#4247=VECTOR('',#15337,1000.);
#4248=VECTOR('',#15340,1000.);
#4249=VECTOR('',#15341,1000.);
#4250=VECTOR('',#15342,1000.);
#4251=VECTOR('',#15345,1000.);
#4252=VECTOR('',#15346,1000.);
#4253=VECTOR('',#15347,1000.);
#4254=VECTOR('',#15350,1000.);
#4255=VECTOR('',#15351,1000.);
#4256=CIRCLE('',#11107,1.25);
#4257=CIRCLE('',#11108,1.25);
#4258=CIRCLE('',#11110,1.25);
#4259=CIRCLE('',#11111,1.25);
#4260=CIRCLE('',#11113,1.25);
#4261=CIRCLE('',#11114,1.25);
#4262=CIRCLE('',#11116,1.25);
#4263=CIRCLE('',#11117,1.25);
#4264=CIRCLE('',#11119,1.25);
#4265=CIRCLE('',#11120,1.25);
#4266=CIRCLE('',#11122,1.25);
#4267=CIRCLE('',#11123,1.25);
#4268=CIRCLE('',#11125,1.25);
#4269=CIRCLE('',#11126,1.25);
#4270=CIRCLE('',#11128,1.25);
#4271=CIRCLE('',#11129,1.25);
#4272=CIRCLE('',#11131,1.24999999999999);
#4273=CIRCLE('',#11132,1.25);
#4274=CIRCLE('',#11134,1.24999999999999);
#4275=CIRCLE('',#11135,1.25);
#4276=CIRCLE('',#11137,1.24999999999999);
#4277=CIRCLE('',#11138,1.25);
#4278=CIRCLE('',#11140,1.24999999999999);
#4279=CIRCLE('',#11141,1.25);
#4280=CIRCLE('',#11143,1.24999999999999);
#4281=CIRCLE('',#11144,1.25);
#4282=CIRCLE('',#11146,1.25);
#4283=CIRCLE('',#11147,1.25);
#4284=CIRCLE('',#11149,1.25000000000001);
#4285=CIRCLE('',#11150,1.25);
#4286=CIRCLE('',#11152,1.25);
#4287=CIRCLE('',#11153,1.25);
#4288=CIRCLE('',#11155,5.);
#4289=CIRCLE('',#11156,5.);
#4290=CIRCLE('',#11158,3.);
#4291=CIRCLE('',#11159,6.);
#4292=CIRCLE('',#11162,3.);
#4293=CIRCLE('',#11163,6.);
#4294=CIRCLE('',#11166,3.);
#4295=CIRCLE('',#11167,6.);
#4296=CIRCLE('',#11170,3.);
#4297=CIRCLE('',#11171,6.);
#4298=CIRCLE('',#11174,2.5);
#4299=CIRCLE('',#11175,2.5);
#4300=CIRCLE('',#11176,2.5);
#4301=CIRCLE('',#11177,2.5);
#4302=CIRCLE('',#11180,2.5);
#4303=CIRCLE('',#11181,2.5);
#4304=CIRCLE('',#11182,2.5);
#4305=CIRCLE('',#11183,2.5);
#4306=CIRCLE('',#11188,2.5);
#4307=CIRCLE('',#11189,2.5);
#4308=CIRCLE('',#11190,2.5);
#4309=CIRCLE('',#11191,2.5);
#4310=CIRCLE('',#11194,2.5);
#4311=CIRCLE('',#11195,2.5);
#4312=CIRCLE('',#11196,2.5);
#4313=CIRCLE('',#11197,2.5);
#4314=CIRCLE('',#11217,5.5);
#4315=CIRCLE('',#11218,5.5);
#4316=CIRCLE('',#11220,14.);
#4317=CIRCLE('',#11221,14.);
#4318=CIRCLE('',#11223,1.35);
#4319=CIRCLE('',#11224,1.35);
#4320=CIRCLE('',#11226,1.35);
#4321=CIRCLE('',#11227,1.35);
#4322=CIRCLE('',#11229,1.35);
#4323=CIRCLE('',#11230,1.35);
#4324=CIRCLE('',#11232,1.35);
#4325=CIRCLE('',#11233,1.35);
#4326=CIRCLE('',#11235,1.35);
#4327=CIRCLE('',#11236,1.35);
#4328=CIRCLE('',#11238,1.35);
#4329=CIRCLE('',#11239,1.35);
#4330=CIRCLE('',#11241,1.35);
#4331=CIRCLE('',#11242,1.35);
#4332=CIRCLE('',#11244,1.35);
#4333=CIRCLE('',#11245,1.35);
#4334=CIRCLE('',#11247,1.35);
#4335=CIRCLE('',#11248,1.35);
#4336=CIRCLE('',#11250,1.35);
#4337=CIRCLE('',#11251,1.35);
#4338=CIRCLE('',#11253,1.35);
#4339=CIRCLE('',#11254,1.35);
#4340=CIRCLE('',#11256,1.35);
#4341=CIRCLE('',#11257,1.35);
#4342=CIRCLE('',#11259,5.);
#4343=CIRCLE('',#11260,5.);
#4344=CIRCLE('',#11262,7.5);
#4345=CIRCLE('',#11263,7.5);
#4346=CIRCLE('',#11265,2.75);
#4347=CIRCLE('',#11266,2.75);
#4348=CIRCLE('',#11268,5.);
#4349=CIRCLE('',#11269,5.);
#4350=CIRCLE('',#11271,7.25);
#4351=CIRCLE('',#11272,7.25);
#4352=CIRCLE('',#11274,14.);
#4353=CIRCLE('',#11275,14.);
#4354=CIRCLE('',#11277,4.75);
#4355=CIRCLE('',#11278,4.75);
#4356=CIRCLE('',#11280,2.75);
#4357=CIRCLE('',#11281,2.75);
#4358=CIRCLE('',#11284,2.);
#4359=CIRCLE('',#11285,2.);
#4360=CIRCLE('',#11287,1.5);
#4361=CIRCLE('',#11288,1.5);
#4362=CIRCLE('',#11290,1.5);
#4363=CIRCLE('',#11291,1.5);
#4364=CIRCLE('',#11293,1.5);
#4365=CIRCLE('',#11294,1.5);
#4366=CIRCLE('',#11297,0.49999972876243);
#4367=CIRCLE('',#11298,1.50000000000168);
#4368=CIRCLE('',#11299,0.499999999994099);
#4369=CIRCLE('',#11300,1.49999999999602);
#4370=CIRCLE('',#11307,2.);
#4371=CIRCLE('',#11308,2.);
#4372=CIRCLE('',#11310,2.);
#4373=CIRCLE('',#11311,2.);
#4374=CIRCLE('',#11313,2.);
#4375=CIRCLE('',#11314,2.);
#4376=CIRCLE('',#11316,3.);
#4377=CIRCLE('',#11317,3.);
#4378=CIRCLE('',#11318,3.);
#4379=CIRCLE('',#11319,3.);
#4380=CIRCLE('',#11320,3.);
#4381=CIRCLE('',#11321,1.5);
#4382=CIRCLE('',#11322,2.35);
#4383=CIRCLE('',#11323,0.999999999999999);
#4384=CIRCLE('',#11324,0.999999999999999);
#4385=CIRCLE('',#11325,2.35);
#4386=CIRCLE('',#11326,1.);
#4387=CIRCLE('',#11327,1.);
#4388=CIRCLE('',#11328,2.35);
#4389=CIRCLE('',#11329,0.999999999999999);
#4390=CIRCLE('',#11330,0.999999999999999);
#4391=CIRCLE('',#11331,2.35);
#4392=CIRCLE('',#11332,1.50000000000001);
#4393=CIRCLE('',#11333,2.);
#4394=CIRCLE('',#11334,3.);
#4395=CIRCLE('',#11336,3.5);
#4396=CIRCLE('',#11337,3.5);
#4397=CIRCLE('',#11339,2.);
#4398=CIRCLE('',#11341,2.);
#4399=CIRCLE('',#11342,2.);
#4400=CIRCLE('',#11344,2.);
#4401=CIRCLE('',#11345,2.);
#4402=CIRCLE('',#11347,1.5);
#4403=CIRCLE('',#11349,1.5);
#4404=CIRCLE('',#11351,3.);
#4405=CIRCLE('',#11352,3.);
#4406=CIRCLE('',#11353,0.999999999999999);
#4407=CIRCLE('',#11354,0.999999999999999);
#4408=CIRCLE('',#11355,3.);
#4409=CIRCLE('',#11356,3.);
#4410=CIRCLE('',#11357,3.);
#4411=CIRCLE('',#11358,3.);
#4412=CIRCLE('',#11360,0.999999999999996);
#4413=CIRCLE('',#11362,0.99999999999999);
#4414=CIRCLE('',#11370,3.);
#4415=CIRCLE('',#11373,3.);
#4416=CIRCLE('',#11376,3.);
#4417=CIRCLE('',#11377,3.);
#4418=CIRCLE('',#11378,3.);
#4419=CIRCLE('',#11381,3.);
#4420=CIRCLE('',#11382,3.);
#4421=CIRCLE('',#11383,3.);
#4422=CIRCLE('',#11386,3.);
#4423=CIRCLE('',#11389,3.);
#4424=CIRCLE('',#11391,1.5);
#4425=CIRCLE('',#11392,2.00000000000001);
#4426=CIRCLE('',#11395,2.35);
#4427=CIRCLE('',#11398,0.999999999999057);
#4428=CIRCLE('',#11401,1.00000000000512);
#4429=CIRCLE('',#11404,2.35);
#4430=CIRCLE('',#11407,0.999999999999075);
#4431=CIRCLE('',#11410,1.00000000000602);
#4432=CIRCLE('',#11413,2.35);
#4433=CIRCLE('',#11416,1.00000000000513);
#4434=CIRCLE('',#11419,1.00000000000602);
#4435=CIRCLE('',#11422,2.35);
#4436=CIRCLE('',#11424,2.00000000000002);
#4437=CIRCLE('',#11426,1.5);
#4438=CIRCLE('',#11429,3.85000089750977);
#4439=CIRCLE('',#11430,3.85000061127743);
#4440=CIRCLE('',#11431,3.84999875153457);
#4441=CIRCLE('',#11432,3.84999771098492);
#4442=CIRCLE('',#11439,3.);
#4443=CIRCLE('',#11442,3.);
#4444=CIRCLE('',#11443,3.);
#4445=CIRCLE('',#11444,3.);
#4446=CIRCLE('',#11447,3.);
#4447=CIRCLE('',#11448,3.);
#4448=CIRCLE('',#11449,3.);
#4449=CIRCLE('',#11452,3.);
#4450=CIRCLE('',#11455,3.);
#4451=CIRCLE('',#11457,3.);
#4452=CIRCLE('',#11463,2.);
#4453=CIRCLE('',#11465,2.);
#4454=CIRCLE('',#11522,1.5);
#4455=CIRCLE('',#11524,1.5);
#4456=CIRCLE('',#11526,1.5);
#4457=CIRCLE('',#11528,1.5);
#4458=CIRCLE('',#11529,1.5);
#4459=CIRCLE('',#11531,1.5);
#4460=CIRCLE('',#11532,1.5);
#4461=CIRCLE('',#11534,1.5);
#4462=CIRCLE('',#11536,1.5);
#4463=CIRCLE('',#11538,1.5);
#4464=CIRCLE('',#11539,1.5);
#4465=CIRCLE('',#11541,1.5);
#4466=CIRCLE('',#11542,1.5);
#4467=CIRCLE('',#11544,1.5);
#4468=CIRCLE('',#11546,1.5);
#4469=CIRCLE('',#11548,1.5);
#4470=CIRCLE('',#11549,1.5);
#4471=CIRCLE('',#11551,1.5);
#4472=CIRCLE('',#11552,1.5);
#4473=CIRCLE('',#11554,1.5);
#4474=CIRCLE('',#11583,2.);
#4475=CIRCLE('',#11585,2.);
#4476=CIRCLE('',#11676,1.25);
#4477=CIRCLE('',#11677,1.25);
#4478=CIRCLE('',#11679,1.25);
#4479=CIRCLE('',#11680,1.25);
#4480=CIRCLE('',#11682,1.25);
#4481=CIRCLE('',#11683,1.25);
#4482=CIRCLE('',#11685,1.25);
#4483=CIRCLE('',#11686,1.25);
#4484=CIRCLE('',#11688,1.025);
#4485=CIRCLE('',#11689,1.025);
#4486=CIRCLE('',#11691,1.025);
#4487=CIRCLE('',#11692,1.025);
#4488=CIRCLE('',#11694,1.025);
#4489=CIRCLE('',#11695,1.025);
#4490=CIRCLE('',#11697,1.025);
#4491=CIRCLE('',#11698,1.025);
#4492=CIRCLE('',#11700,1.25);
#4493=CIRCLE('',#11701,1.25);
#4494=CIRCLE('',#11703,1.25);
#4495=CIRCLE('',#11704,1.25);
#4496=CIRCLE('',#11706,1.25);
#4497=CIRCLE('',#11707,1.25);
#4498=CIRCLE('',#11709,1.25);
#4499=CIRCLE('',#11710,1.25);
#4500=CIRCLE('',#11712,1.025);
#4501=CIRCLE('',#11713,1.025);
#4502=CIRCLE('',#11715,1.025);
#4503=CIRCLE('',#11716,1.025);
#4504=CIRCLE('',#11718,1.025);
#4505=CIRCLE('',#11719,1.025);
#4506=CIRCLE('',#11721,1.025);
#4507=CIRCLE('',#11722,1.025);
#4508=CIRCLE('',#11724,1.25);
#4509=CIRCLE('',#11725,1.25);
#4510=CIRCLE('',#11727,1.25);
#4511=CIRCLE('',#11728,1.25);
#4512=CIRCLE('',#11730,1.25);
#4513=CIRCLE('',#11731,1.25);
#4514=CIRCLE('',#11733,1.25);
#4515=CIRCLE('',#11734,1.25);
#4516=CIRCLE('',#11736,1.25);
#4517=CIRCLE('',#11737,1.25);
#4518=CIRCLE('',#11739,1.25);
#4519=CIRCLE('',#11740,1.25);
#4520=CIRCLE('',#11742,1.25);
#4521=CIRCLE('',#11743,1.25);
#4522=CIRCLE('',#11745,1.25);
#4523=CIRCLE('',#11746,1.25);
#4524=CIRCLE('',#11748,5.);
#4525=CIRCLE('',#11749,5.);
#4526=CIRCLE('',#11751,1.35000000003038);
#4527=CIRCLE('',#11753,1.35000000003038);
#4528=CIRCLE('',#11755,1.35000000003038);
#4529=CIRCLE('',#11757,1.35000000003038);
#4530=CIRCLE('',#11759,1.35000000002083);
#4531=CIRCLE('',#11761,1.35000000002083);
#4532=CIRCLE('',#11763,1.35000000002083);
#4533=CIRCLE('',#11765,1.35000000002083);
#4534=CIRCLE('',#11767,5.19994989682595);
#4535=CIRCLE('',#11769,1.3);
#4536=CIRCLE('',#11770,1.3);
#4537=CIRCLE('',#11772,1.3);
#4538=CIRCLE('',#11773,1.3);
#4539=CIRCLE('',#11775,1.3);
#4540=CIRCLE('',#11776,1.3);
#4541=CIRCLE('',#11778,1.3);
#4542=CIRCLE('',#11779,1.3);
#4543=CIRCLE('',#11781,1.3);
#4544=CIRCLE('',#11782,1.3);
#4545=CIRCLE('',#11784,1.3);
#4546=CIRCLE('',#11785,1.3);
#4547=CIRCLE('',#11787,1.3);
#4548=CIRCLE('',#11788,1.3);
#4549=CIRCLE('',#11790,1.3);
#4550=CIRCLE('',#11791,1.3);
#4551=CIRCLE('',#11793,6.);
#4552=CIRCLE('',#11794,6.);
#4553=CIRCLE('',#11796,0.5);
#4554=CIRCLE('',#11799,2.5);
#4555=CIRCLE('',#11800,2.5);
#4556=CIRCLE('',#11801,0.5);
#4557=CIRCLE('',#11805,6.);
#4558=CIRCLE('',#11808,6.);
#4559=CIRCLE('',#11811,2.);
#4560=CIRCLE('',#11812,2.);
#4561=CIRCLE('',#11813,2.);
#4562=CIRCLE('',#11815,2.);
#4563=CIRCLE('',#11816,2.);
#4564=CIRCLE('',#11817,2.);
#4565=CIRCLE('',#11819,4.05035655858838);
#4566=CIRCLE('',#11821,4.0503565587057);
#4567=CIRCLE('',#11824,2.);
#4568=CIRCLE('',#11826,2.);
#4569=CIRCLE('',#11829,2.);
#4570=CIRCLE('',#11832,2.);
#4571=CIRCLE('',#11834,2.);
#4572=CIRCLE('',#11837,2.);
#4573=CIRCLE('',#11843,1.25);
#4574=CIRCLE('',#11844,1.25);
#4575=CIRCLE('',#11846,1.25);
#4576=CIRCLE('',#11847,1.25);
#4577=CIRCLE('',#11849,1.25);
#4578=CIRCLE('',#11850,1.25);
#4579=CIRCLE('',#11852,1.25);
#4580=CIRCLE('',#11853,1.25);
#4581=CIRCLE('',#11855,1.25);
#4582=CIRCLE('',#11856,1.25);
#4583=CIRCLE('',#11858,1.25);
#4584=CIRCLE('',#11859,1.25);
#4585=CIRCLE('',#11861,1.25);
#4586=CIRCLE('',#11862,1.25);
#4587=CIRCLE('',#11864,1.25);
#4588=CIRCLE('',#11865,1.25);
#4589=CIRCLE('',#11868,2.5);
#4590=CIRCLE('',#11869,4.59);
#4591=CIRCLE('',#11870,2.5);
#4592=CIRCLE('',#11872,1.25);
#4593=CIRCLE('',#11873,1.25);
#4594=CIRCLE('',#11875,1.25);
#4595=CIRCLE('',#11876,1.25);
#4596=CIRCLE('',#11878,1.25);
#4597=CIRCLE('',#11879,1.25);
#4598=CIRCLE('',#11881,1.25);
#4599=CIRCLE('',#11882,1.25);
#4600=CIRCLE('',#11884,1.25);
#4601=CIRCLE('',#11885,1.25);
#4602=CIRCLE('',#11887,1.25);
#4603=CIRCLE('',#11888,1.25);
#4604=CIRCLE('',#11890,1.25);
#4605=CIRCLE('',#11891,1.25);
#4606=CIRCLE('',#11893,1.25);
#4607=CIRCLE('',#11894,1.25);
#4608=CIRCLE('',#11896,5.5);
#4609=CIRCLE('',#11897,5.5);
#4610=CIRCLE('',#11899,2.5);
#4611=CIRCLE('',#11901,14.);
#4612=CIRCLE('',#11902,9.);
#4613=CIRCLE('',#11904,14.);
#4614=CIRCLE('',#11905,9.);
#4615=CIRCLE('',#11913,12.5);
#4616=CIRCLE('',#11914,12.5);
#4617=CIRCLE('',#11916,12.5);
#4618=CIRCLE('',#11917,12.5);
#4619=CIRCLE('',#11919,12.5);
#4620=CIRCLE('',#11920,12.5);
#4621=CIRCLE('',#11922,12.);
#4622=CIRCLE('',#11923,12.);
#4623=CIRCLE('',#11925,8.);
#4624=CIRCLE('',#11926,8.);
#4625=CIRCLE('',#11928,8.);
#4626=CIRCLE('',#11929,8.);
#4627=CIRCLE('',#11938,12.);
#4628=CIRCLE('',#11939,12.);
#4629=CIRCLE('',#11943,10.);
#4630=CIRCLE('',#11944,10.);
#4631=CIRCLE('',#11945,10.);
#4632=CIRCLE('',#11947,10.);
#4633=CIRCLE('',#11948,10.);
#4634=CIRCLE('',#11949,10.);
#4635=CIRCLE('',#11966,8.);
#4636=CIRCLE('',#11967,8.00000000000001);
#4637=CIRCLE('',#11969,1.25);
#4638=CIRCLE('',#11970,1.25);
#4639=CIRCLE('',#11972,1.25);
#4640=CIRCLE('',#11973,1.25);
#4641=CIRCLE('',#11975,1.25);
#4642=CIRCLE('',#11976,1.25);
#4643=CIRCLE('',#11978,1.25);
#4644=CIRCLE('',#11979,1.25);
#4645=CIRCLE('',#11994,12.);
#4646=CIRCLE('',#11995,12.);
#4647=CIRCLE('',#11999,10.);
#4648=CIRCLE('',#12000,10.);
#4649=CIRCLE('',#12002,10.);
#4650=CIRCLE('',#12003,10.);
#4651=CIRCLE('',#12012,5.51648351648352);
#4652=CIRCLE('',#12013,1.21175743903915);
#4653=CIRCLE('',#12014,5.51648351648352);
#4654=CIRCLE('',#12016,4.);
#4655=CIRCLE('',#12017,4.25);
#4656=CIRCLE('',#12019,4.);
#4657=CIRCLE('',#12020,4.);
#4658=CIRCLE('',#12022,4.25);
#4659=CIRCLE('',#12024,5.51648351648352);
#4660=CIRCLE('',#12026,5.51648351648352);
#4661=CIRCLE('',#12030,1.21175743903915);
#4662=CIRCLE('',#12032,1.21175743903915);
#4663=CIRCLE('',#12034,1.21175743903915);
#4664=CIRCLE('',#12036,1.21175743903915);
#4665=CIRCLE('',#12038,1.21175743903915);
#4666=CIRCLE('',#12040,1.21175743903915);
#4667=CIRCLE('',#12042,1.21175743903915);
#4668=CIRCLE('',#12044,1.21175743903915);
#4669=CIRCLE('',#12046,1.21175743903915);
#4670=CIRCLE('',#12048,1.21175743903915);
#4671=CIRCLE('',#12050,1.21175743903915);
#4672=CIRCLE('',#12052,1.21175743903915);
#4673=CIRCLE('',#12054,6.48351648351648);
#4674=CIRCLE('',#12055,6.48351648351648);
#4675=CIRCLE('',#12057,5.51648351648352);
#4676=CIRCLE('',#12058,5.51648351648352);
#4677=CIRCLE('',#12062,6.48351648351649);
#4678=CIRCLE('',#12063,6.48351648351649);
#4679=CIRCLE('',#12065,5.51648351648352);
#4680=CIRCLE('',#12066,5.51648351648352);
#4681=CIRCLE('',#12070,9.);
#4682=CIRCLE('',#12071,9.);
#4683=CIRCLE('',#12073,6.48351648351648);
#4684=CIRCLE('',#12074,6.48351648351648);
#4685=CIRCLE('',#12076,6.48351648351648);
#4686=CIRCLE('',#12077,1.21175743903915);
#4687=CIRCLE('',#12079,6.48351648351649);
#4688=CIRCLE('',#12081,8.);
#4689=CIRCLE('',#12082,8.);
#4690=CIRCLE('',#12083,8.);
#4691=CIRCLE('',#12085,7.75);
#4692=CIRCLE('',#12091,5.);
#4693=CIRCLE('',#12092,5.);
#4694=CIRCLE('',#12094,2.1);
#4695=CIRCLE('',#12095,2.1);
#4696=CIRCLE('',#12097,4.);
#4697=CIRCLE('',#12098,4.);
#4698=CIRCLE('',#12104,5.);
#4699=CIRCLE('',#12105,5.);
#4700=CIRCLE('',#12107,1.6);
#4701=CIRCLE('',#12108,1.6);
#4702=CIRCLE('',#12110,4.);
#4703=CIRCLE('',#12111,4.);
#4704=CIRCLE('',#12132,2.24999999999999);
#4705=CIRCLE('',#12133,4.59);
#4706=CIRCLE('',#12135,2.24999999999999);
#4707=CIRCLE('',#12137,2.24999999999999);
#4708=CIRCLE('',#12138,4.59);
#4709=CIRCLE('',#12140,2.24999999999999);
#4710=CIRCLE('',#12142,10.);
#4711=CIRCLE('',#12143,10.);
#4712=CIRCLE('',#12145,10.);
#4713=CIRCLE('',#12147,10.);
#4714=CIRCLE('',#12153,1.25);
#4715=CIRCLE('',#12154,1.25);
#4716=CIRCLE('',#12155,1.25);
#4717=CIRCLE('',#12156,1.25);
#4718=CIRCLE('',#12157,1.25);
#4719=CIRCLE('',#12158,1.25);
#4720=CIRCLE('',#12160,2.05857864376269);
#4721=CIRCLE('',#12161,0.2);
#4722=CIRCLE('',#12162,2.);
#4723=CIRCLE('',#12164,3.9);
#4724=CIRCLE('',#12165,3.9);
#4725=CIRCLE('',#12168,2.);
#4726=CIRCLE('',#12170,1.61);
#4727=VERTEX_POINT('',#15425);
#4728=VERTEX_POINT('',#15427);
#4729=VERTEX_POINT('',#15431);
#4730=VERTEX_POINT('',#15433);
#4731=VERTEX_POINT('',#15437);
#4732=VERTEX_POINT('',#15439);
#4733=VERTEX_POINT('',#15443);
#4734=VERTEX_POINT('',#15445);
#4735=VERTEX_POINT('',#15449);
#4736=VERTEX_POINT('',#15451);
#4737=VERTEX_POINT('',#15455);
#4738=VERTEX_POINT('',#15457);
#4739=VERTEX_POINT('',#15461);
#4740=VERTEX_POINT('',#15463);
#4741=VERTEX_POINT('',#15467);
#4742=VERTEX_POINT('',#15469);
#4743=VERTEX_POINT('',#15473);
#4744=VERTEX_POINT('',#15475);
#4745=VERTEX_POINT('',#15479);
#4746=VERTEX_POINT('',#15481);
#4747=VERTEX_POINT('',#15485);
#4748=VERTEX_POINT('',#15487);
#4749=VERTEX_POINT('',#15491);
#4750=VERTEX_POINT('',#15493);
#4751=VERTEX_POINT('',#15497);
#4752=VERTEX_POINT('',#15499);
#4753=VERTEX_POINT('',#15503);
#4754=VERTEX_POINT('',#15505);
#4755=VERTEX_POINT('',#15509);
#4756=VERTEX_POINT('',#15511);
#4757=VERTEX_POINT('',#15515);
#4758=VERTEX_POINT('',#15517);
#4759=VERTEX_POINT('',#15521);
#4760=VERTEX_POINT('',#15523);
#4761=VERTEX_POINT('',#15527);
#4762=VERTEX_POINT('',#15528);
#4763=VERTEX_POINT('',#15530);
#4764=VERTEX_POINT('',#15532);
#4765=VERTEX_POINT('',#15536);
#4766=VERTEX_POINT('',#15538);
#4767=VERTEX_POINT('',#15542);
#4768=VERTEX_POINT('',#15543);
#4769=VERTEX_POINT('',#15545);
#4770=VERTEX_POINT('',#15547);
#4771=VERTEX_POINT('',#15551);
#4772=VERTEX_POINT('',#15553);
#4773=VERTEX_POINT('',#15557);
#4774=VERTEX_POINT('',#15558);
#4775=VERTEX_POINT('',#15563);
#4776=VERTEX_POINT('',#15565);
#4777=VERTEX_POINT('',#15569);
#4778=VERTEX_POINT('',#15570);
#4779=VERTEX_POINT('',#15572);
#4780=VERTEX_POINT('',#15574);
#4781=VERTEX_POINT('',#15581);
#4782=VERTEX_POINT('',#15582);
#4783=VERTEX_POINT('',#15586);
#4784=VERTEX_POINT('',#15588);
#4785=VERTEX_POINT('',#15590);
#4786=VERTEX_POINT('',#15592);
#4787=VERTEX_POINT('',#15594);
#4788=VERTEX_POINT('',#15598);
#4789=VERTEX_POINT('',#15599);
#4790=VERTEX_POINT('',#15604);
#4791=VERTEX_POINT('',#15606);
#4792=VERTEX_POINT('',#15609);
#4793=VERTEX_POINT('',#15611);
#4794=VERTEX_POINT('',#15613);
#4795=VERTEX_POINT('',#15624);
#4796=VERTEX_POINT('',#15626);
#4797=VERTEX_POINT('',#15628);
#4798=VERTEX_POINT('',#15630);
#4799=VERTEX_POINT('',#15632);
#4800=VERTEX_POINT('',#15634);
#4801=VERTEX_POINT('',#15636);
#4802=VERTEX_POINT('',#15640);
#4803=VERTEX_POINT('',#15642);
#4804=VERTEX_POINT('',#15646);
#4805=VERTEX_POINT('',#15647);
#4806=VERTEX_POINT('',#15651);
#4807=VERTEX_POINT('',#15653);
#4808=VERTEX_POINT('',#15655);
#4809=VERTEX_POINT('',#15690);
#4810=VERTEX_POINT('',#15692);
#4811=VERTEX_POINT('',#15696);
#4812=VERTEX_POINT('',#15698);
#4813=VERTEX_POINT('',#15702);
#4814=VERTEX_POINT('',#15704);
#4815=VERTEX_POINT('',#15708);
#4816=VERTEX_POINT('',#15710);
#4817=VERTEX_POINT('',#15714);
#4818=VERTEX_POINT('',#15716);
#4819=VERTEX_POINT('',#15720);
#4820=VERTEX_POINT('',#15722);
#4821=VERTEX_POINT('',#15726);
#4822=VERTEX_POINT('',#15728);
#4823=VERTEX_POINT('',#15732);
#4824=VERTEX_POINT('',#15734);
#4825=VERTEX_POINT('',#15738);
#4826=VERTEX_POINT('',#15740);
#4827=VERTEX_POINT('',#15744);
#4828=VERTEX_POINT('',#15746);
#4829=VERTEX_POINT('',#15750);
#4830=VERTEX_POINT('',#15752);
#4831=VERTEX_POINT('',#15756);
#4832=VERTEX_POINT('',#15758);
#4833=VERTEX_POINT('',#15762);
#4834=VERTEX_POINT('',#15764);
#4835=VERTEX_POINT('',#15768);
#4836=VERTEX_POINT('',#15770);
#4837=VERTEX_POINT('',#15774);
#4838=VERTEX_POINT('',#15776);
#4839=VERTEX_POINT('',#15780);
#4840=VERTEX_POINT('',#15782);
#4841=VERTEX_POINT('',#15786);
#4842=VERTEX_POINT('',#15788);
#4843=VERTEX_POINT('',#15792);
#4844=VERTEX_POINT('',#15794);
#4845=VERTEX_POINT('',#15798);
#4846=VERTEX_POINT('',#15800);
#4847=VERTEX_POINT('',#15804);
#4848=VERTEX_POINT('',#15806);
#4849=VERTEX_POINT('',#15810);
#4850=VERTEX_POINT('',#15812);
#4851=VERTEX_POINT('',#15816);
#4852=VERTEX_POINT('',#15818);
#4853=VERTEX_POINT('',#15822);
#4854=VERTEX_POINT('',#15823);
#4855=VERTEX_POINT('',#15825);
#4856=VERTEX_POINT('',#15827);
#4857=VERTEX_POINT('',#15831);
#4858=VERTEX_POINT('',#15833);
#4859=VERTEX_POINT('',#15837);
#4860=VERTEX_POINT('',#15838);
#4861=VERTEX_POINT('',#15843);
#4862=VERTEX_POINT('',#15844);
#4863=VERTEX_POINT('',#15849);
#4864=VERTEX_POINT('',#15851);
#4865=VERTEX_POINT('',#15856);
#4866=VERTEX_POINT('',#15858);
#4867=VERTEX_POINT('',#15860);
#4868=VERTEX_POINT('',#15862);
#4869=VERTEX_POINT('',#15864);
#4870=VERTEX_POINT('',#15866);
#4871=VERTEX_POINT('',#15868);
#4872=VERTEX_POINT('',#15870);
#4873=VERTEX_POINT('',#15872);
#4874=VERTEX_POINT('',#15874);
#4875=VERTEX_POINT('',#15876);
#4876=VERTEX_POINT('',#15878);
#4877=VERTEX_POINT('',#15880);
#4878=VERTEX_POINT('',#15882);
#4879=VERTEX_POINT('',#15884);
#4880=VERTEX_POINT('',#15886);
#4881=VERTEX_POINT('',#15904);
#4882=VERTEX_POINT('',#15922);
#4883=VERTEX_POINT('',#15926);
#4884=VERTEX_POINT('',#15927);
#4885=VERTEX_POINT('',#15929);
#4886=VERTEX_POINT('',#16119);
#4887=VERTEX_POINT('',#16120);
#4888=VERTEX_POINT('',#16174);
#4889=VERTEX_POINT('',#16179);
#4890=VERTEX_POINT('',#16238);
#4891=VERTEX_POINT('',#16240);
#4892=VERTEX_POINT('',#16242);
#4893=VERTEX_POINT('',#16297);
#4894=VERTEX_POINT('',#16298);
#4895=VERTEX_POINT('',#16303);
#4896=VERTEX_POINT('',#16304);
#4897=VERTEX_POINT('',#16309);
#4898=VERTEX_POINT('',#16310);
#4899=VERTEX_POINT('',#16315);
#4900=VERTEX_POINT('',#16316);
#4901=VERTEX_POINT('',#16318);
#4902=VERTEX_POINT('',#16320);
#4903=VERTEX_POINT('',#16322);
#4904=VERTEX_POINT('',#16324);
#4905=VERTEX_POINT('',#16326);
#4906=VERTEX_POINT('',#16328);
#4907=VERTEX_POINT('',#16330);
#4908=VERTEX_POINT('',#16332);
#4909=VERTEX_POINT('',#16334);
#4910=VERTEX_POINT('',#16337);
#4911=VERTEX_POINT('',#16339);
#4912=VERTEX_POINT('',#16341);
#4913=VERTEX_POINT('',#16343);
#4914=VERTEX_POINT('',#16345);
#4915=VERTEX_POINT('',#16347);
#4916=VERTEX_POINT('',#16349);
#4917=VERTEX_POINT('',#16351);
#4918=VERTEX_POINT('',#16353);
#4919=VERTEX_POINT('',#16355);
#4920=VERTEX_POINT('',#16357);
#4921=VERTEX_POINT('',#16359);
#4922=VERTEX_POINT('',#16361);
#4923=VERTEX_POINT('',#16363);
#4924=VERTEX_POINT('',#16365);
#4925=VERTEX_POINT('',#16367);
#4926=VERTEX_POINT('',#16369);
#4927=VERTEX_POINT('',#16371);
#4928=VERTEX_POINT('',#16373);
#4929=VERTEX_POINT('',#16375);
#4930=VERTEX_POINT('',#16377);
#4931=VERTEX_POINT('',#16379);
#4932=VERTEX_POINT('',#16382);
#4933=VERTEX_POINT('',#16384);
#4934=VERTEX_POINT('',#16388);
#4935=VERTEX_POINT('',#16390);
#4936=VERTEX_POINT('',#16394);
#4937=VERTEX_POINT('',#16398);
#4938=VERTEX_POINT('',#16400);
#4939=VERTEX_POINT('',#16404);
#4940=VERTEX_POINT('',#16406);
#4941=VERTEX_POINT('',#16414);
#4942=VERTEX_POINT('',#16415);
#4943=VERTEX_POINT('',#16417);
#4944=VERTEX_POINT('',#16419);
#4945=VERTEX_POINT('',#16424);
#4946=VERTEX_POINT('',#16426);
#4947=VERTEX_POINT('',#16428);
#4948=VERTEX_POINT('',#16430);
#4949=VERTEX_POINT('',#16432);
#4950=VERTEX_POINT('',#16434);
#4951=VERTEX_POINT('',#16436);
#4952=VERTEX_POINT('',#16438);
#4953=VERTEX_POINT('',#16535);
#4954=VERTEX_POINT('',#16536);
#4955=VERTEX_POINT('',#16538);
#4956=VERTEX_POINT('',#16541);
#4957=VERTEX_POINT('',#16543);
#4958=VERTEX_POINT('',#16547);
#4959=VERTEX_POINT('',#16551);
#4960=VERTEX_POINT('',#16552);
#4961=VERTEX_POINT('',#16554);
#4962=VERTEX_POINT('',#16556);
#4963=VERTEX_POINT('',#16558);
#4964=VERTEX_POINT('',#16560);
#4965=VERTEX_POINT('',#16562);
#4966=VERTEX_POINT('',#16564);
#4967=VERTEX_POINT('',#16566);
#4968=VERTEX_POINT('',#16568);
#4969=VERTEX_POINT('',#16570);
#4970=VERTEX_POINT('',#16572);
#4971=VERTEX_POINT('',#16574);
#4972=VERTEX_POINT('',#16576);
#4973=VERTEX_POINT('',#16578);
#4974=VERTEX_POINT('',#16581);
#4975=VERTEX_POINT('',#16583);
#4976=VERTEX_POINT('',#16585);
#4977=VERTEX_POINT('',#16587);
#4978=VERTEX_POINT('',#16589);
#4979=VERTEX_POINT('',#16591);
#4980=VERTEX_POINT('',#16593);
#4981=VERTEX_POINT('',#16595);
#4982=VERTEX_POINT('',#16597);
#4983=VERTEX_POINT('',#16599);
#4984=VERTEX_POINT('',#16601);
#4985=VERTEX_POINT('',#16603);
#4986=VERTEX_POINT('',#16605);
#4987=VERTEX_POINT('',#16607);
#4988=VERTEX_POINT('',#16609);
#4989=VERTEX_POINT('',#16611);
#4990=VERTEX_POINT('',#16613);
#4991=VERTEX_POINT('',#16615);
#4992=VERTEX_POINT('',#16617);
#4993=VERTEX_POINT('',#16619);
#4994=VERTEX_POINT('',#16621);
#4995=VERTEX_POINT('',#16623);
#4996=VERTEX_POINT('',#16627);
#4997=VERTEX_POINT('',#16631);
#4998=VERTEX_POINT('',#16632);
#4999=VERTEX_POINT('',#16634);
#5000=VERTEX_POINT('',#16636);
#5001=VERTEX_POINT('',#16641);
#5002=VERTEX_POINT('',#16643);
#5003=VERTEX_POINT('',#16647);
#5004=VERTEX_POINT('',#16649);
#5005=VERTEX_POINT('',#16651);
#5006=VERTEX_POINT('',#16653);
#5007=VERTEX_POINT('',#16655);
#5008=VERTEX_POINT('',#16657);
#5009=VERTEX_POINT('',#16659);
#5010=VERTEX_POINT('',#16661);
#5011=VERTEX_POINT('',#16663);
#5012=VERTEX_POINT('',#16665);
#5013=VERTEX_POINT('',#16667);
#5014=VERTEX_POINT('',#16669);
#5015=VERTEX_POINT('',#16671);
#5016=VERTEX_POINT('',#16675);
#5017=VERTEX_POINT('',#16679);
#5018=VERTEX_POINT('',#16683);
#5019=VERTEX_POINT('',#16684);
#5020=VERTEX_POINT('',#16686);
#5021=VERTEX_POINT('',#16691);
#5022=VERTEX_POINT('',#16693);
#5023=VERTEX_POINT('',#16695);
#5024=VERTEX_POINT('',#16697);
#5025=VERTEX_POINT('',#16699);
#5026=VERTEX_POINT('',#16701);
#5027=VERTEX_POINT('',#16703);
#5028=VERTEX_POINT('',#16705);
#5029=VERTEX_POINT('',#16707);
#5030=VERTEX_POINT('',#16711);
#5031=VERTEX_POINT('',#16713);
#5032=VERTEX_POINT('',#16718);
#5033=VERTEX_POINT('',#16722);
#5034=VERTEX_POINT('',#16726);
#5035=VERTEX_POINT('',#16728);
#5036=VERTEX_POINT('',#16730);
#5037=VERTEX_POINT('',#16732);
#5038=VERTEX_POINT('',#16734);
#5039=VERTEX_POINT('',#16736);
#5040=VERTEX_POINT('',#16738);
#5041=VERTEX_POINT('',#16740);
#5042=VERTEX_POINT('',#16742);
#5043=VERTEX_POINT('',#16744);
#5044=VERTEX_POINT('',#16746);
#5045=VERTEX_POINT('',#16748);
#5046=VERTEX_POINT('',#16750);
#5047=VERTEX_POINT('',#16756);
#5048=VERTEX_POINT('',#16760);
#5049=VERTEX_POINT('',#16764);
#5050=VERTEX_POINT('',#16768);
#5051=VERTEX_POINT('',#16769);
#5052=VERTEX_POINT('',#16777);
#5053=VERTEX_POINT('',#16781);
#5054=VERTEX_POINT('',#16786);
#5055=VERTEX_POINT('',#16788);
#5056=VERTEX_POINT('',#16795);
#5057=VERTEX_POINT('',#16799);
#5058=VERTEX_POINT('',#16801);
#5059=VERTEX_POINT('',#16808);
#5060=VERTEX_POINT('',#16812);
#5061=VERTEX_POINT('',#16813);
#5062=VERTEX_POINT('',#16821);
#5063=VERTEX_POINT('',#16825);
#5064=VERTEX_POINT('',#16830);
#5065=VERTEX_POINT('',#16832);
#5066=VERTEX_POINT('',#16839);
#5067=VERTEX_POINT('',#16843);
#5068=VERTEX_POINT('',#16845);
#5069=VERTEX_POINT('',#16852);
#5070=VERTEX_POINT('',#16856);
#5071=VERTEX_POINT('',#16857);
#5072=VERTEX_POINT('',#16865);
#5073=VERTEX_POINT('',#16869);
#5074=VERTEX_POINT('',#16874);
#5075=VERTEX_POINT('',#16876);
#5076=VERTEX_POINT('',#16883);
#5077=VERTEX_POINT('',#16887);
#5078=VERTEX_POINT('',#16889);
#5079=VERTEX_POINT('',#16896);
#5080=VERTEX_POINT('',#16900);
#5081=VERTEX_POINT('',#16906);
#5082=VERTEX_POINT('',#16908);
#5083=VERTEX_POINT('',#16910);
#5084=VERTEX_POINT('',#16912);
#5085=VERTEX_POINT('',#16916);
#5086=VERTEX_POINT('',#16917);
#5087=VERTEX_POINT('',#16919);
#5088=VERTEX_POINT('',#16921);
#5089=VERTEX_POINT('',#16923);
#5090=VERTEX_POINT('',#16925);
#5091=VERTEX_POINT('',#16927);
#5092=VERTEX_POINT('',#16929);
#5093=VERTEX_POINT('',#16931);
#5094=VERTEX_POINT('',#16933);
#5095=VERTEX_POINT('',#16935);
#5096=VERTEX_POINT('',#16937);
#5097=VERTEX_POINT('',#16939);
#5098=VERTEX_POINT('',#16941);
#5099=VERTEX_POINT('',#16946);
#5100=VERTEX_POINT('',#16950);
#5101=VERTEX_POINT('',#16952);
#5102=VERTEX_POINT('',#16956);
#5103=VERTEX_POINT('',#16957);
#5104=VERTEX_POINT('',#16959);
#5105=VERTEX_POINT('',#16961);
#5106=VERTEX_POINT('',#16963);
#5107=VERTEX_POINT('',#16965);
#5108=VERTEX_POINT('',#16967);
#5109=VERTEX_POINT('',#16969);
#5110=VERTEX_POINT('',#16971);
#5111=VERTEX_POINT('',#16974);
#5112=VERTEX_POINT('',#16976);
#5113=VERTEX_POINT('',#16978);
#5114=VERTEX_POINT('',#16980);
#5115=VERTEX_POINT('',#16982);
#5116=VERTEX_POINT('',#16984);
#5117=VERTEX_POINT('',#16986);
#5118=VERTEX_POINT('',#16988);
#5119=VERTEX_POINT('',#16990);
#5120=VERTEX_POINT('',#16992);
#5121=VERTEX_POINT('',#16994);
#5122=VERTEX_POINT('',#16996);
#5123=VERTEX_POINT('',#16998);
#5124=VERTEX_POINT('',#17000);
#5125=VERTEX_POINT('',#17002);
#5126=VERTEX_POINT('',#17004);
#5127=VERTEX_POINT('',#17006);
#5128=VERTEX_POINT('',#17009);
#5129=VERTEX_POINT('',#17011);
#5130=VERTEX_POINT('',#17013);
#5131=VERTEX_POINT('',#17015);
#5132=VERTEX_POINT('',#17017);
#5133=VERTEX_POINT('',#17019);
#5134=VERTEX_POINT('',#17021);
#5135=VERTEX_POINT('',#17023);
#5136=VERTEX_POINT('',#17025);
#5137=VERTEX_POINT('',#17029);
#5138=VERTEX_POINT('',#17031);
#5139=VERTEX_POINT('',#17033);
#5140=VERTEX_POINT('',#17035);
#5141=VERTEX_POINT('',#17039);
#5142=VERTEX_POINT('',#17040);
#5143=VERTEX_POINT('',#17042);
#5144=VERTEX_POINT('',#17045);
#5145=VERTEX_POINT('',#17047);
#5146=VERTEX_POINT('',#17049);
#5147=VERTEX_POINT('',#17051);
#5148=VERTEX_POINT('',#17053);
#5149=VERTEX_POINT('',#17055);
#5150=VERTEX_POINT('',#17057);
#5151=VERTEX_POINT('',#17059);
#5152=VERTEX_POINT('',#17061);
#5153=VERTEX_POINT('',#17063);
#5154=VERTEX_POINT('',#17065);
#5155=VERTEX_POINT('',#17069);
#5156=VERTEX_POINT('',#17073);
#5157=VERTEX_POINT('',#17077);
#5158=VERTEX_POINT('',#17079);
#5159=VERTEX_POINT('',#17084);
#5160=VERTEX_POINT('',#17085);
#5161=VERTEX_POINT('',#17088);
#5162=VERTEX_POINT('',#17090);
#5163=VERTEX_POINT('',#17092);
#5164=VERTEX_POINT('',#17094);
#5165=VERTEX_POINT('',#17096);
#5166=VERTEX_POINT('',#17098);
#5167=VERTEX_POINT('',#17100);
#5168=VERTEX_POINT('',#17104);
#5169=VERTEX_POINT('',#17107);
#5170=VERTEX_POINT('',#17111);
#5171=VERTEX_POINT('',#17115);
#5172=VERTEX_POINT('',#17119);
#5173=VERTEX_POINT('',#17120);
#5174=VERTEX_POINT('',#17123);
#5175=VERTEX_POINT('',#17125);
#5176=VERTEX_POINT('',#17127);
#5177=VERTEX_POINT('',#17129);
#5178=VERTEX_POINT('',#17131);
#5179=VERTEX_POINT('',#17133);
#5180=VERTEX_POINT('',#17135);
#5181=VERTEX_POINT('',#17137);
#5182=VERTEX_POINT('',#17139);
#5183=VERTEX_POINT('',#17141);
#5184=VERTEX_POINT('',#17143);
#5185=VERTEX_POINT('',#17151);
#5186=VERTEX_POINT('',#17153);
#5187=VERTEX_POINT('',#17161);
#5188=VERTEX_POINT('',#17166);
#5189=VERTEX_POINT('',#17167);
#5190=VERTEX_POINT('',#17170);
#5191=VERTEX_POINT('',#17174);
#5192=VERTEX_POINT('',#17178);
#5193=VERTEX_POINT('',#17180);
#5194=VERTEX_POINT('',#17182);
#5195=VERTEX_POINT('',#17190);
#5196=VERTEX_POINT('',#17192);
#5197=VERTEX_POINT('',#17196);
#5198=VERTEX_POINT('',#17200);
#5199=VERTEX_POINT('',#17202);
#5200=VERTEX_POINT('',#17206);
#5201=VERTEX_POINT('',#17210);
#5202=VERTEX_POINT('',#17214);
#5203=VERTEX_POINT('',#17215);
#5204=VERTEX_POINT('',#17220);
#5205=VERTEX_POINT('',#17223);
#5206=VERTEX_POINT('',#17227);
#5207=VERTEX_POINT('',#17232);
#5208=VERTEX_POINT('',#17242);
#5209=VERTEX_POINT('',#17246);
#5210=VERTEX_POINT('',#17251);
#5211=VERTEX_POINT('',#17256);
#5212=VERTEX_POINT('',#17261);
#5213=VERTEX_POINT('',#17271);
#5214=VERTEX_POINT('',#17275);
#5215=VERTEX_POINT('',#17280);
#5216=VERTEX_POINT('',#17288);
#5217=VERTEX_POINT('',#17292);
#5218=VERTEX_POINT('',#17294);
#5219=VERTEX_POINT('',#17296);
#5220=VERTEX_POINT('',#17300);
#5221=VERTEX_POINT('',#17302);
#5222=VERTEX_POINT('',#17304);
#5223=VERTEX_POINT('',#17308);
#5224=VERTEX_POINT('',#17310);
#5225=VERTEX_POINT('',#17312);
#5226=VERTEX_POINT('',#17316);
#5227=VERTEX_POINT('',#17318);
#5228=VERTEX_POINT('',#17320);
#5229=VERTEX_POINT('',#17324);
#5230=VERTEX_POINT('',#17326);
#5231=VERTEX_POINT('',#17328);
#5232=VERTEX_POINT('',#17332);
#5233=VERTEX_POINT('',#17334);
#5234=VERTEX_POINT('',#17338);
#5235=VERTEX_POINT('',#17349);
#5236=VERTEX_POINT('',#17353);
#5237=VERTEX_POINT('',#17357);
#5238=VERTEX_POINT('',#17359);
#5239=VERTEX_POINT('',#17363);
#5240=VERTEX_POINT('',#17369);
#5241=VERTEX_POINT('',#17373);
#5242=VERTEX_POINT('',#17375);
#5243=VERTEX_POINT('',#17379);
#5244=VERTEX_POINT('',#17383);
#5245=VERTEX_POINT('',#17387);
#5246=VERTEX_POINT('',#17436);
#5247=VERTEX_POINT('',#17448);
#5248=VERTEX_POINT('',#17452);
#5249=VERTEX_POINT('',#17457);
#5250=VERTEX_POINT('',#17467);
#5251=VERTEX_POINT('',#17471);
#5252=VERTEX_POINT('',#17475);
#5253=VERTEX_POINT('',#17479);
#5254=VERTEX_POINT('',#17487);
#5255=VERTEX_POINT('',#17492);
#5256=VERTEX_POINT('',#17496);
#5257=VERTEX_POINT('',#17500);
#5258=VERTEX_POINT('',#17502);
#5259=VERTEX_POINT('',#17506);
#5260=VERTEX_POINT('',#17510);
#5261=VERTEX_POINT('',#17514);
#5262=VERTEX_POINT('',#17518);
#5263=VERTEX_POINT('',#17522);
#5264=VERTEX_POINT('',#17524);
#5265=VERTEX_POINT('',#17526);
#5266=VERTEX_POINT('',#17530);
#5267=VERTEX_POINT('',#17534);
#5268=VERTEX_POINT('',#17536);
#5269=VERTEX_POINT('',#17538);
#5270=VERTEX_POINT('',#17546);
#5271=VERTEX_POINT('',#17550);
#5272=VERTEX_POINT('',#17552);
#5273=VERTEX_POINT('',#17554);
#5274=VERTEX_POINT('',#17558);
#5275=VERTEX_POINT('',#17559);
#5276=VERTEX_POINT('',#17562);
#5277=VERTEX_POINT('',#17566);
#5278=VERTEX_POINT('',#17568);
#5279=VERTEX_POINT('',#17572);
#5280=VERTEX_POINT('',#17574);
#5281=VERTEX_POINT('',#17576);
#5282=VERTEX_POINT('',#17580);
#5283=VERTEX_POINT('',#17581);
#5284=VERTEX_POINT('',#17584);
#5285=VERTEX_POINT('',#17588);
#5286=VERTEX_POINT('',#17590);
#5287=VERTEX_POINT('',#17600);
#5288=VERTEX_POINT('',#17604);
#5289=VERTEX_POINT('',#17606);
#5290=VERTEX_POINT('',#17610);
#5291=VERTEX_POINT('',#17614);
#5292=VERTEX_POINT('',#17618);
#5293=VERTEX_POINT('',#17633);
#5294=VERTEX_POINT('',#17637);
#5295=VERTEX_POINT('',#17639);
#5296=VERTEX_POINT('',#17642);
#5297=VERTEX_POINT('',#17645);
#5298=VERTEX_POINT('',#17650);
#5299=VERTEX_POINT('',#17659);
#5300=VERTEX_POINT('',#17660);
#5301=VERTEX_POINT('',#17662);
#5302=VERTEX_POINT('',#17664);
#5303=VERTEX_POINT('',#17681);
#5304=VERTEX_POINT('',#18420);
#5305=VERTEX_POINT('',#18421);
#5306=VERTEX_POINT('',#18423);
#5307=VERTEX_POINT('',#18425);
#5308=VERTEX_POINT('',#18432);
#5309=VERTEX_POINT('',#18448);
#5310=VERTEX_POINT('',#18449);
#5311=VERTEX_POINT('',#18454);
#5312=VERTEX_POINT('',#18458);
#5313=VERTEX_POINT('',#18728);
#5314=VERTEX_POINT('',#18729);
#5315=VERTEX_POINT('',#18734);
#5316=VERTEX_POINT('',#18738);
#5317=VERTEX_POINT('',#18753);
#5318=VERTEX_POINT('',#18755);
#5319=VERTEX_POINT('',#18759);
#5320=VERTEX_POINT('',#18761);
#5321=VERTEX_POINT('',#18765);
#5322=VERTEX_POINT('',#18767);
#5323=VERTEX_POINT('',#18771);
#5324=VERTEX_POINT('',#18773);
#5325=VERTEX_POINT('',#18777);
#5326=VERTEX_POINT('',#18779);
#5327=VERTEX_POINT('',#18783);
#5328=VERTEX_POINT('',#18785);
#5329=VERTEX_POINT('',#18789);
#5330=VERTEX_POINT('',#18791);
#5331=VERTEX_POINT('',#18795);
#5332=VERTEX_POINT('',#18797);
#5333=VERTEX_POINT('',#18801);
#5334=VERTEX_POINT('',#18803);
#5335=VERTEX_POINT('',#18807);
#5336=VERTEX_POINT('',#18809);
#5337=VERTEX_POINT('',#18813);
#5338=VERTEX_POINT('',#18815);
#5339=VERTEX_POINT('',#18819);
#5340=VERTEX_POINT('',#18821);
#5341=VERTEX_POINT('',#18825);
#5342=VERTEX_POINT('',#18827);
#5343=VERTEX_POINT('',#18831);
#5344=VERTEX_POINT('',#18833);
#5345=VERTEX_POINT('',#18837);
#5346=VERTEX_POINT('',#18839);
#5347=VERTEX_POINT('',#18843);
#5348=VERTEX_POINT('',#18845);
#5349=VERTEX_POINT('',#18849);
#5350=VERTEX_POINT('',#18851);
#5351=VERTEX_POINT('',#18855);
#5352=VERTEX_POINT('',#18857);
#5353=VERTEX_POINT('',#18861);
#5354=VERTEX_POINT('',#18863);
#5355=VERTEX_POINT('',#18867);
#5356=VERTEX_POINT('',#18869);
#5357=VERTEX_POINT('',#18873);
#5358=VERTEX_POINT('',#18875);
#5359=VERTEX_POINT('',#18879);
#5360=VERTEX_POINT('',#18881);
#5361=VERTEX_POINT('',#18885);
#5362=VERTEX_POINT('',#18887);
#5363=VERTEX_POINT('',#18891);
#5364=VERTEX_POINT('',#18893);
#5365=VERTEX_POINT('',#18897);
#5366=VERTEX_POINT('',#18899);
#5367=VERTEX_POINT('',#18903);
#5368=VERTEX_POINT('',#18907);
#5369=VERTEX_POINT('',#18911);
#5370=VERTEX_POINT('',#18915);
#5371=VERTEX_POINT('',#18919);
#5372=VERTEX_POINT('',#18923);
#5373=VERTEX_POINT('',#18927);
#5374=VERTEX_POINT('',#18931);
#5375=VERTEX_POINT('',#18935);
#5376=VERTEX_POINT('',#18939);
#5377=VERTEX_POINT('',#18941);
#5378=VERTEX_POINT('',#18945);
#5379=VERTEX_POINT('',#18947);
#5380=VERTEX_POINT('',#18951);
#5381=VERTEX_POINT('',#18953);
#5382=VERTEX_POINT('',#18957);
#5383=VERTEX_POINT('',#18959);
#5384=VERTEX_POINT('',#18963);
#5385=VERTEX_POINT('',#18965);
#5386=VERTEX_POINT('',#18969);
#5387=VERTEX_POINT('',#18971);
#5388=VERTEX_POINT('',#18975);
#5389=VERTEX_POINT('',#18977);
#5390=VERTEX_POINT('',#18981);
#5391=VERTEX_POINT('',#18983);
#5392=VERTEX_POINT('',#18987);
#5393=VERTEX_POINT('',#18988);
#5394=VERTEX_POINT('',#18990);
#5395=VERTEX_POINT('',#18992);
#5396=VERTEX_POINT('',#18994);
#5397=VERTEX_POINT('',#18996);
#5398=VERTEX_POINT('',#19000);
#5399=VERTEX_POINT('',#19002);
#5400=VERTEX_POINT('',#19017);
#5401=VERTEX_POINT('',#19021);
#5402=VERTEX_POINT('',#19023);
#5403=VERTEX_POINT('',#19025);
#5404=VERTEX_POINT('',#19027);
#5405=VERTEX_POINT('',#19029);
#5406=VERTEX_POINT('',#19031);
#5407=VERTEX_POINT('',#19033);
#5408=VERTEX_POINT('',#19035);
#5409=VERTEX_POINT('',#19037);
#5410=VERTEX_POINT('',#19041);
#5411=VERTEX_POINT('',#19043);
#5412=VERTEX_POINT('',#19060);
#5413=VERTEX_POINT('',#19062);
#5414=VERTEX_POINT('',#19064);
#5415=VERTEX_POINT('',#19068);
#5416=VERTEX_POINT('',#19072);
#5417=VERTEX_POINT('',#19074);
#5418=VERTEX_POINT('',#19081);
#5419=VERTEX_POINT('',#19083);
#5420=VERTEX_POINT('',#19085);
#5421=VERTEX_POINT('',#19087);
#5422=VERTEX_POINT('',#19089);
#5423=VERTEX_POINT('',#19128);
#5424=VERTEX_POINT('',#19180);
#5425=VERTEX_POINT('',#19197);
#5426=VERTEX_POINT('',#19198);
#5427=VERTEX_POINT('',#19200);
#5428=VERTEX_POINT('',#19202);
#5429=VERTEX_POINT('',#19205);
#5430=VERTEX_POINT('',#19209);
#5431=VERTEX_POINT('',#19213);
#5432=VERTEX_POINT('',#19217);
#5433=VERTEX_POINT('',#19220);
#5434=VERTEX_POINT('',#19224);
#5435=VERTEX_POINT('',#19228);
#5436=VERTEX_POINT('',#19230);
#5437=VERTEX_POINT('',#19234);
#5438=VERTEX_POINT('',#19287);
#5439=VERTEX_POINT('',#19291);
#5440=VERTEX_POINT('',#19293);
#5441=VERTEX_POINT('',#19297);
#5442=VERTEX_POINT('',#19301);
#5443=VERTEX_POINT('',#19303);
#5444=VERTEX_POINT('',#19317);
#5445=VERTEX_POINT('',#19319);
#5446=VERTEX_POINT('',#19323);
#5447=VERTEX_POINT('',#19325);
#5448=VERTEX_POINT('',#19329);
#5449=VERTEX_POINT('',#19331);
#5450=VERTEX_POINT('',#19335);
#5451=VERTEX_POINT('',#19337);
#5452=VERTEX_POINT('',#19341);
#5453=VERTEX_POINT('',#19343);
#5454=VERTEX_POINT('',#19347);
#5455=VERTEX_POINT('',#19349);
#5456=VERTEX_POINT('',#19353);
#5457=VERTEX_POINT('',#19355);
#5458=VERTEX_POINT('',#19359);
#5459=VERTEX_POINT('',#19361);
#5460=VERTEX_POINT('',#19366);
#5461=VERTEX_POINT('',#19367);
#5462=VERTEX_POINT('',#19369);
#5463=VERTEX_POINT('',#19374);
#5464=VERTEX_POINT('',#19376);
#5465=VERTEX_POINT('',#19380);
#5466=VERTEX_POINT('',#19382);
#5467=VERTEX_POINT('',#19386);
#5468=VERTEX_POINT('',#19388);
#5469=VERTEX_POINT('',#19392);
#5470=VERTEX_POINT('',#19394);
#5471=VERTEX_POINT('',#19398);
#5472=VERTEX_POINT('',#19400);
#5473=VERTEX_POINT('',#19404);
#5474=VERTEX_POINT('',#19406);
#5475=VERTEX_POINT('',#19410);
#5476=VERTEX_POINT('',#19412);
#5477=VERTEX_POINT('',#19416);
#5478=VERTEX_POINT('',#19418);
#5479=VERTEX_POINT('',#19422);
#5480=VERTEX_POINT('',#19424);
#5481=VERTEX_POINT('',#19428);
#5482=VERTEX_POINT('',#19432);
#5483=VERTEX_POINT('',#19433);
#5484=VERTEX_POINT('',#19435);
#5485=VERTEX_POINT('',#19437);
#5486=VERTEX_POINT('',#19441);
#5487=VERTEX_POINT('',#19442);
#5488=VERTEX_POINT('',#19444);
#5489=VERTEX_POINT('',#19446);
#5490=VERTEX_POINT('',#19460);
#5491=VERTEX_POINT('',#19462);
#5492=VERTEX_POINT('',#19466);
#5493=VERTEX_POINT('',#19468);
#5494=VERTEX_POINT('',#19472);
#5495=VERTEX_POINT('',#19474);
#5496=VERTEX_POINT('',#19478);
#5497=VERTEX_POINT('',#19479);
#5498=VERTEX_POINT('',#19481);
#5499=VERTEX_POINT('',#19483);
#5500=VERTEX_POINT('',#19487);
#5501=VERTEX_POINT('',#19489);
#5502=VERTEX_POINT('',#19493);
#5503=VERTEX_POINT('',#19495);
#5504=VERTEX_POINT('',#19499);
#5505=VERTEX_POINT('',#19500);
#5506=VERTEX_POINT('',#19502);
#5507=VERTEX_POINT('',#19504);
#5508=VERTEX_POINT('',#19506);
#5509=VERTEX_POINT('',#19508);
#5510=VERTEX_POINT('',#19510);
#5511=VERTEX_POINT('',#19512);
#5512=VERTEX_POINT('',#19514);
#5513=VERTEX_POINT('',#19516);
#5514=VERTEX_POINT('',#19520);
#5515=VERTEX_POINT('',#19522);
#5516=VERTEX_POINT('',#19526);
#5517=VERTEX_POINT('',#19528);
#5518=VERTEX_POINT('',#19532);
#5519=VERTEX_POINT('',#19533);
#5520=VERTEX_POINT('',#19535);
#5521=VERTEX_POINT('',#19537);
#5522=VERTEX_POINT('',#19541);
#5523=VERTEX_POINT('',#19543);
#5524=VERTEX_POINT('',#19547);
#5525=VERTEX_POINT('',#19549);
#5526=VERTEX_POINT('',#19551);
#5527=VERTEX_POINT('',#19553);
#5528=VERTEX_POINT('',#19559);
#5529=VERTEX_POINT('',#19560);
#5530=VERTEX_POINT('',#19562);
#5531=VERTEX_POINT('',#19564);
#5532=VERTEX_POINT('',#19574);
#5533=VERTEX_POINT('',#19580);
#5534=VERTEX_POINT('',#19595);
#5535=VERTEX_POINT('',#19596);
#5536=VERTEX_POINT('',#19598);
#5537=VERTEX_POINT('',#19600);
#5538=VERTEX_POINT('',#19604);
#5539=VERTEX_POINT('',#19606);
#5540=VERTEX_POINT('',#19610);
#5541=VERTEX_POINT('',#19612);
#5542=VERTEX_POINT('',#19623);
#5543=VERTEX_POINT('',#19625);
#5544=VERTEX_POINT('',#19629);
#5545=VERTEX_POINT('',#19631);
#5546=VERTEX_POINT('',#19635);
#5547=VERTEX_POINT('',#19637);
#5548=VERTEX_POINT('',#19641);
#5549=VERTEX_POINT('',#19643);
#5550=VERTEX_POINT('',#19647);
#5551=VERTEX_POINT('',#19649);
#5552=VERTEX_POINT('',#19653);
#5553=VERTEX_POINT('',#19654);
#5554=VERTEX_POINT('',#19656);
#5555=VERTEX_POINT('',#19658);
#5556=VERTEX_POINT('',#19662);
#5557=VERTEX_POINT('',#19663);
#5558=VERTEX_POINT('',#19666);
#5559=VERTEX_POINT('',#19668);
#5560=VERTEX_POINT('',#19672);
#5561=VERTEX_POINT('',#19674);
#5562=VERTEX_POINT('',#19678);
#5563=VERTEX_POINT('',#19679);
#5564=VERTEX_POINT('',#19681);
#5565=VERTEX_POINT('',#19684);
#5566=VERTEX_POINT('',#19688);
#5567=VERTEX_POINT('',#19689);
#5568=VERTEX_POINT('',#19694);
#5569=VERTEX_POINT('',#19695);
#5570=VERTEX_POINT('',#19697);
#5571=VERTEX_POINT('',#19699);
#5572=VERTEX_POINT('',#19704);
#5573=VERTEX_POINT('',#19705);
#5574=VERTEX_POINT('',#19707);
#5575=VERTEX_POINT('',#19709);
#5576=VERTEX_POINT('',#19714);
#5577=VERTEX_POINT('',#19716);
#5578=VERTEX_POINT('',#19718);
#5579=VERTEX_POINT('',#19720);
#5580=VERTEX_POINT('',#19726);
#5581=VERTEX_POINT('',#19727);
#5582=VERTEX_POINT('',#19732);
#5583=VERTEX_POINT('',#19734);
#5584=VERTEX_POINT('',#19742);
#5585=VERTEX_POINT('',#19743);
#5586=VERTEX_POINT('',#19745);
#5587=VERTEX_POINT('',#19747);
#5588=VERTEX_POINT('',#19751);
#5589=VERTEX_POINT('',#19753);
#5590=VERTEX_POINT('',#19757);
#5591=VERTEX_POINT('',#19759);
#5592=VERTEX_POINT('',#19780);
#5593=VERTEX_POINT('',#19782);
#5594=VERTEX_POINT('',#19786);
#5595=VERTEX_POINT('',#19788);
#5596=VERTEX_POINT('',#19792);
#5597=VERTEX_POINT('',#19793);
#5598=VERTEX_POINT('',#19798);
#5599=VERTEX_POINT('',#19802);
#5600=VERTEX_POINT('',#19806);
#5601=VERTEX_POINT('',#19812);
#5602=VERTEX_POINT('',#19813);
#5603=VERTEX_POINT('',#19816);
#5604=VERTEX_POINT('',#19817);
#5605=VERTEX_POINT('',#19820);
#5606=VERTEX_POINT('',#19821);
#5607=VERTEX_POINT('',#19824);
#5608=VERTEX_POINT('',#19825);
#5609=VERTEX_POINT('',#19828);
#5610=VERTEX_POINT('',#19829);
#5611=VERTEX_POINT('',#19832);
#5612=VERTEX_POINT('',#19833);
#5613=VERTEX_POINT('',#19836);
#5614=VERTEX_POINT('',#19837);
#5615=VERTEX_POINT('',#19840);
#5616=VERTEX_POINT('',#19841);
#5617=VERTEX_POINT('',#19844);
#5618=VERTEX_POINT('',#19845);
#5619=VERTEX_POINT('',#19848);
#5620=VERTEX_POINT('',#19849);
#5621=VERTEX_POINT('',#19852);
#5622=VERTEX_POINT('',#19853);
#5623=VERTEX_POINT('',#19856);
#5624=VERTEX_POINT('',#19857);
#5625=VERTEX_POINT('',#19860);
#5626=VERTEX_POINT('',#19862);
#5627=VERTEX_POINT('',#19866);
#5628=VERTEX_POINT('',#19868);
#5629=VERTEX_POINT('',#19874);
#5630=VERTEX_POINT('',#19876);
#5631=VERTEX_POINT('',#19880);
#5632=VERTEX_POINT('',#19882);
#5633=VERTEX_POINT('',#19888);
#5634=VERTEX_POINT('',#19890);
#5635=VERTEX_POINT('',#19894);
#5636=VERTEX_POINT('',#19896);
#5637=VERTEX_POINT('',#19900);
#5638=VERTEX_POINT('',#19904);
#5639=VERTEX_POINT('',#19908);
#5640=VERTEX_POINT('',#19909);
#5641=VERTEX_POINT('',#19912);
#5642=VERTEX_POINT('',#19916);
#5643=VERTEX_POINT('',#19924);
#5644=VERTEX_POINT('',#19926);
#5645=VERTEX_POINT('',#19930);
#5646=VERTEX_POINT('',#19932);
#5647=VERTEX_POINT('',#19936);
#5648=VERTEX_POINT('',#19938);
#5649=VERTEX_POINT('',#19946);
#5650=VERTEX_POINT('',#19948);
#5651=VERTEX_POINT('',#19952);
#5652=VERTEX_POINT('',#19954);
#5653=VERTEX_POINT('',#19958);
#5654=VERTEX_POINT('',#19960);
#5655=VERTEX_POINT('',#19983);
#5656=VERTEX_POINT('',#19985);
#5657=VERTEX_POINT('',#19989);
#5658=VERTEX_POINT('',#19993);
#5659=VERTEX_POINT('',#19995);
#5660=VERTEX_POINT('',#19999);
#5661=VERTEX_POINT('',#20003);
#5662=VERTEX_POINT('',#20004);
#5663=VERTEX_POINT('',#20006);
#5664=VERTEX_POINT('',#20008);
#5665=VERTEX_POINT('',#20012);
#5666=VERTEX_POINT('',#20013);
#5667=VERTEX_POINT('',#20018);
#5668=VERTEX_POINT('',#20019);
#5669=VERTEX_POINT('',#20030);
#5670=VERTEX_POINT('',#20031);
#5671=VERTEX_POINT('',#20033);
#5672=VERTEX_POINT('',#20035);
#5673=VERTEX_POINT('',#20037);
#5674=VERTEX_POINT('',#20039);
#5675=VERTEX_POINT('',#20041);
#5676=VERTEX_POINT('',#20045);
#5677=VERTEX_POINT('',#20047);
#5678=VERTEX_POINT('',#20051);
#5679=VERTEX_POINT('',#20053);
#5680=VERTEX_POINT('',#20059);
#5681=VERTEX_POINT('',#20063);
#5682=VERTEX_POINT('',#20067);
#5683=VERTEX_POINT('',#20068);
#5684=VERTEX_POINT('',#20070);
#5685=VERTEX_POINT('',#20072);
#5686=VERTEX_POINT('',#20074);
#5687=VERTEX_POINT('',#20076);
#5688=VERTEX_POINT('',#20081);
#5689=VERTEX_POINT('',#20084);
#5690=VERTEX_POINT('',#20089);
#5691=VERTEX_POINT('',#20094);
#5692=VERTEX_POINT('',#20099);
#5693=VERTEX_POINT('',#20104);
#5694=EDGE_CURVE('',#4727,#4727,#4256,.T.);
#5695=EDGE_CURVE('',#4727,#4728,#2280,.T.);
#5696=EDGE_CURVE('',#4728,#4728,#4257,.T.);
#5697=EDGE_CURVE('',#4729,#4729,#4258,.T.);
#5698=EDGE_CURVE('',#4729,#4730,#2281,.T.);
#5699=EDGE_CURVE('',#4730,#4730,#4259,.T.);
#5700=EDGE_CURVE('',#4731,#4731,#4260,.T.);
#5701=EDGE_CURVE('',#4731,#4732,#2282,.T.);
#5702=EDGE_CURVE('',#4732,#4732,#4261,.T.);
#5703=EDGE_CURVE('',#4733,#4733,#4262,.T.);
#5704=EDGE_CURVE('',#4733,#4734,#2283,.T.);
#5705=EDGE_CURVE('',#4734,#4734,#4263,.T.);
#5706=EDGE_CURVE('',#4735,#4735,#4264,.T.);
#5707=EDGE_CURVE('',#4735,#4736,#2284,.T.);
#5708=EDGE_CURVE('',#4736,#4736,#4265,.T.);
#5709=EDGE_CURVE('',#4737,#4737,#4266,.T.);
#5710=EDGE_CURVE('',#4737,#4738,#2285,.T.);
#5711=EDGE_CURVE('',#4738,#4738,#4267,.T.);
#5712=EDGE_CURVE('',#4739,#4739,#4268,.T.);
#5713=EDGE_CURVE('',#4739,#4740,#2286,.T.);
#5714=EDGE_CURVE('',#4740,#4740,#4269,.T.);
#5715=EDGE_CURVE('',#4741,#4741,#4270,.T.);
#5716=EDGE_CURVE('',#4741,#4742,#2287,.T.);
#5717=EDGE_CURVE('',#4742,#4742,#4271,.T.);
#5718=EDGE_CURVE('',#4743,#4743,#4272,.T.);
#5719=EDGE_CURVE('',#4743,#4744,#2288,.T.);
#5720=EDGE_CURVE('',#4744,#4744,#4273,.T.);
#5721=EDGE_CURVE('',#4745,#4745,#4274,.T.);
#5722=EDGE_CURVE('',#4745,#4746,#2289,.T.);
#5723=EDGE_CURVE('',#4746,#4746,#4275,.T.);
#5724=EDGE_CURVE('',#4747,#4747,#4276,.T.);
#5725=EDGE_CURVE('',#4747,#4748,#2290,.T.);
#5726=EDGE_CURVE('',#4748,#4748,#4277,.T.);
#5727=EDGE_CURVE('',#4749,#4749,#4278,.T.);
#5728=EDGE_CURVE('',#4749,#4750,#2291,.T.);
#5729=EDGE_CURVE('',#4750,#4750,#4279,.T.);
#5730=EDGE_CURVE('',#4751,#4751,#4280,.T.);
#5731=EDGE_CURVE('',#4751,#4752,#2292,.T.);
#5732=EDGE_CURVE('',#4752,#4752,#4281,.T.);
#5733=EDGE_CURVE('',#4753,#4753,#4282,.T.);
#5734=EDGE_CURVE('',#4753,#4754,#2293,.T.);
#5735=EDGE_CURVE('',#4754,#4754,#4283,.T.);
#5736=EDGE_CURVE('',#4755,#4755,#4284,.T.);
#5737=EDGE_CURVE('',#4755,#4756,#2294,.T.);
#5738=EDGE_CURVE('',#4756,#4756,#4285,.T.);
#5739=EDGE_CURVE('',#4757,#4757,#4286,.T.);
#5740=EDGE_CURVE('',#4757,#4758,#2295,.T.);
#5741=EDGE_CURVE('',#4758,#4758,#4287,.T.);
#5742=EDGE_CURVE('',#4759,#4759,#4288,.T.);
#5743=EDGE_CURVE('',#4759,#4760,#2296,.T.);
#5744=EDGE_CURVE('',#4760,#4760,#4289,.T.);
#5745=EDGE_CURVE('',#4761,#4762,#2297,.T.);
#5746=EDGE_CURVE('',#4763,#4761,#4290,.T.);
#5747=EDGE_CURVE('',#4764,#4763,#2298,.T.);
#5748=EDGE_CURVE('',#4764,#4762,#4291,.T.);
#5749=EDGE_CURVE('',#4761,#4765,#2299,.T.);
#5750=EDGE_CURVE('',#4762,#4766,#2300,.T.);
#5751=EDGE_CURVE('',#4766,#4765,#2301,.T.);
#5752=EDGE_CURVE('',#4767,#4768,#2302,.T.);
#5753=EDGE_CURVE('',#4767,#4769,#4292,.T.);
#5754=EDGE_CURVE('',#4770,#4769,#2303,.T.);
#5755=EDGE_CURVE('',#4768,#4770,#4293,.T.);
#5756=EDGE_CURVE('',#4771,#4768,#2304,.T.);
#5757=EDGE_CURVE('',#4771,#4772,#2305,.T.);
#5758=EDGE_CURVE('',#4772,#4767,#2306,.T.);
#5759=EDGE_CURVE('',#4773,#4774,#2307,.T.);
#5760=EDGE_CURVE('',#4765,#4773,#4294,.T.);
#5761=EDGE_CURVE('',#4766,#4774,#4295,.T.);
#5762=EDGE_CURVE('',#4774,#4775,#2308,.T.);
#5763=EDGE_CURVE('',#4775,#4776,#2309,.T.);
#5764=EDGE_CURVE('',#4773,#4776,#2310,.T.);
#5765=EDGE_CURVE('',#4777,#4778,#2311,.T.);
#5766=EDGE_CURVE('',#4777,#4779,#4296,.T.);
#5767=EDGE_CURVE('',#4780,#4779,#2312,.T.);
#5768=EDGE_CURVE('',#4778,#4780,#4297,.T.);
#5769=EDGE_CURVE('',#4769,#4777,#2313,.T.);
#5770=EDGE_CURVE('',#4770,#4778,#2314,.T.);
#5771=EDGE_CURVE('',#4781,#4782,#2315,.T.);
#5772=EDGE_CURVE('',#4782,#4775,#4298,.T.);
#5773=EDGE_CURVE('',#4774,#4780,#2316,.T.);
#5774=EDGE_CURVE('',#4780,#4783,#2317,.T.);
#5775=EDGE_CURVE('',#4783,#4784,#4299,.T.);
#5776=EDGE_CURVE('',#4784,#4785,#2318,.T.);
#5777=EDGE_CURVE('',#4785,#4786,#4300,.T.);
#5778=EDGE_CURVE('',#4787,#4786,#2319,.T.);
#5779=EDGE_CURVE('',#4787,#4781,#4301,.T.);
#5780=EDGE_CURVE('',#4788,#4789,#2320,.T.);
#5781=EDGE_CURVE('',#4788,#4787,#2321,.T.);
#5782=EDGE_CURVE('',#4786,#4789,#2322,.T.);
#5783=EDGE_CURVE('',#4776,#4790,#4302,.T.);
#5784=EDGE_CURVE('',#4790,#4791,#2323,.T.);
#5785=EDGE_CURVE('',#4791,#4788,#4303,.T.);
#5786=EDGE_CURVE('',#4789,#4792,#4304,.T.);
#5787=EDGE_CURVE('',#4792,#4793,#2324,.T.);
#5788=EDGE_CURVE('',#4793,#4794,#4305,.T.);
#5789=EDGE_CURVE('',#4779,#4794,#2325,.T.);
#5790=EDGE_CURVE('',#4773,#4779,#2326,.T.);
#5791=EDGE_CURVE('',#4765,#4777,#2327,.T.);
#5792=EDGE_CURVE('',#4761,#4769,#2328,.T.);
#5793=EDGE_CURVE('',#4763,#4767,#2329,.T.);
#5794=EDGE_CURVE('',#4772,#4795,#4306,.T.);
#5795=EDGE_CURVE('',#4795,#4796,#2330,.T.);
#5796=EDGE_CURVE('',#4796,#4797,#4307,.T.);
#5797=EDGE_CURVE('',#4798,#4797,#2331,.T.);
#5798=EDGE_CURVE('',#4798,#4799,#4308,.T.);
#5799=EDGE_CURVE('',#4799,#4800,#2332,.T.);
#5800=EDGE_CURVE('',#4800,#4801,#4309,.T.);
#5801=EDGE_CURVE('',#4801,#4763,#2333,.T.);
#5802=EDGE_CURVE('',#4797,#4802,#2334,.T.);
#5803=EDGE_CURVE('',#4803,#4802,#2335,.T.);
#5804=EDGE_CURVE('',#4803,#4798,#2336,.T.);
#5805=EDGE_CURVE('',#4804,#4805,#2337,.T.);
#5806=EDGE_CURVE('',#4805,#4771,#4310,.T.);
#5807=EDGE_CURVE('',#4764,#4768,#2338,.T.);
#5808=EDGE_CURVE('',#4806,#4764,#2339,.T.);
#5809=EDGE_CURVE('',#4806,#4807,#4311,.T.);
#5810=EDGE_CURVE('',#4807,#4808,#2340,.T.);
#5811=EDGE_CURVE('',#4808,#4803,#4312,.T.);
#5812=EDGE_CURVE('',#4802,#4804,#4313,.T.);
#5813=EDGE_CURVE('',#4762,#4770,#2341,.T.);
#5814=EDGE_CURVE('',#4766,#4778,#2342,.T.);
#5815=EDGE_CURVE('',#4801,#4806,#2343,.T.);
#5816=EDGE_CURVE('',#4794,#4783,#2344,.T.);
#5817=EDGE_CURVE('',#4792,#4785,#2345,.T.);
#5818=EDGE_CURVE('',#4784,#4793,#2346,.T.);
#5819=EDGE_CURVE('',#4795,#4805,#2347,.T.);
#5820=EDGE_CURVE('',#4804,#4796,#2348,.T.);
#5821=EDGE_CURVE('',#4790,#4782,#2349,.T.);
#5822=EDGE_CURVE('',#4781,#4791,#2350,.T.);
#5823=EDGE_CURVE('',#4807,#4800,#2351,.T.);
#5824=EDGE_CURVE('',#4799,#4808,#2352,.T.);
#5825=EDGE_CURVE('',#4809,#4809,#4314,.T.);
#5826=EDGE_CURVE('',#4809,#4810,#2353,.T.);
#5827=EDGE_CURVE('',#4810,#4810,#4315,.T.);
#5828=EDGE_CURVE('',#4811,#4811,#4316,.T.);
#5829=EDGE_CURVE('',#4811,#4812,#2354,.T.);
#5830=EDGE_CURVE('',#4812,#4812,#4317,.T.);
#5831=EDGE_CURVE('',#4813,#4813,#4318,.T.);
#5832=EDGE_CURVE('',#4813,#4814,#2355,.T.);
#5833=EDGE_CURVE('',#4814,#4814,#4319,.T.);
#5834=EDGE_CURVE('',#4815,#4815,#4320,.T.);
#5835=EDGE_CURVE('',#4815,#4816,#2356,.T.);
#5836=EDGE_CURVE('',#4816,#4816,#4321,.T.);
#5837=EDGE_CURVE('',#4817,#4817,#4322,.T.);
#5838=EDGE_CURVE('',#4817,#4818,#2357,.T.);
#5839=EDGE_CURVE('',#4818,#4818,#4323,.T.);
#5840=EDGE_CURVE('',#4819,#4819,#4324,.T.);
#5841=EDGE_CURVE('',#4819,#4820,#2358,.T.);
#5842=EDGE_CURVE('',#4820,#4820,#4325,.T.);
#5843=EDGE_CURVE('',#4821,#4821,#4326,.T.);
#5844=EDGE_CURVE('',#4821,#4822,#2359,.T.);
#5845=EDGE_CURVE('',#4822,#4822,#4327,.T.);
#5846=EDGE_CURVE('',#4823,#4823,#4328,.T.);
#5847=EDGE_CURVE('',#4823,#4824,#2360,.T.);
#5848=EDGE_CURVE('',#4824,#4824,#4329,.T.);
#5849=EDGE_CURVE('',#4825,#4825,#4330,.T.);
#5850=EDGE_CURVE('',#4825,#4826,#2361,.T.);
#5851=EDGE_CURVE('',#4826,#4826,#4331,.T.);
#5852=EDGE_CURVE('',#4827,#4827,#4332,.T.);
#5853=EDGE_CURVE('',#4827,#4828,#2362,.T.);
#5854=EDGE_CURVE('',#4828,#4828,#4333,.T.);
#5855=EDGE_CURVE('',#4829,#4829,#4334,.T.);
#5856=EDGE_CURVE('',#4829,#4830,#2363,.T.);
#5857=EDGE_CURVE('',#4830,#4830,#4335,.T.);
#5858=EDGE_CURVE('',#4831,#4831,#4336,.T.);
#5859=EDGE_CURVE('',#4831,#4832,#2364,.T.);
#5860=EDGE_CURVE('',#4832,#4832,#4337,.T.);
#5861=EDGE_CURVE('',#4833,#4833,#4338,.T.);
#5862=EDGE_CURVE('',#4833,#4834,#2365,.T.);
#5863=EDGE_CURVE('',#4834,#4834,#4339,.T.);
#5864=EDGE_CURVE('',#4835,#4835,#4340,.T.);
#5865=EDGE_CURVE('',#4835,#4836,#2366,.T.);
#5866=EDGE_CURVE('',#4836,#4836,#4341,.T.);
#5867=EDGE_CURVE('',#4837,#4837,#4342,.T.);
#5868=EDGE_CURVE('',#4837,#4838,#2367,.T.);
#5869=EDGE_CURVE('',#4838,#4838,#4343,.T.);
#5870=EDGE_CURVE('',#4839,#4839,#4344,.T.);
#5871=EDGE_CURVE('',#4839,#4840,#2368,.T.);
#5872=EDGE_CURVE('',#4840,#4840,#4345,.T.);
#5873=EDGE_CURVE('',#4841,#4841,#4346,.T.);
#5874=EDGE_CURVE('',#4841,#4842,#2369,.T.);
#5875=EDGE_CURVE('',#4842,#4842,#4347,.T.);
#5876=EDGE_CURVE('',#4843,#4843,#4348,.T.);
#5877=EDGE_CURVE('',#4843,#4844,#2370,.T.);
#5878=EDGE_CURVE('',#4844,#4844,#4349,.T.);
#5879=EDGE_CURVE('',#4845,#4845,#4350,.T.);
#5880=EDGE_CURVE('',#4845,#4846,#2371,.T.);
#5881=EDGE_CURVE('',#4846,#4846,#4351,.T.);
#5882=EDGE_CURVE('',#4847,#4847,#4352,.T.);
#5883=EDGE_CURVE('',#4847,#4848,#2372,.T.);
#5884=EDGE_CURVE('',#4848,#4848,#4353,.T.);
#5885=EDGE_CURVE('',#4849,#4849,#4354,.T.);
#5886=EDGE_CURVE('',#4849,#4850,#2373,.T.);
#5887=EDGE_CURVE('',#4850,#4850,#4355,.T.);
#5888=EDGE_CURVE('',#4851,#4851,#4356,.T.);
#5889=EDGE_CURVE('',#4851,#4852,#2374,.T.);
#5890=EDGE_CURVE('',#4852,#4852,#4357,.T.);
#5891=EDGE_CURVE('',#4853,#4854,#2375,.T.);
#5892=EDGE_CURVE('',#4854,#4855,#2376,.T.);
#5893=EDGE_CURVE('',#4855,#4856,#2377,.T.);
#5894=EDGE_CURVE('',#4856,#4853,#2378,.T.);
#5895=EDGE_CURVE('',#4854,#4857,#4358,.T.);
#5896=EDGE_CURVE('',#4857,#4858,#2379,.T.);
#5897=EDGE_CURVE('',#4858,#4855,#4359,.T.);
#5898=EDGE_CURVE('',#4859,#4860,#2380,.T.);
#5899=EDGE_CURVE('',#4860,#4854,#4360,.T.);
#5900=EDGE_CURVE('',#4853,#4859,#4361,.T.);
#5901=EDGE_CURVE('',#4861,#4862,#2381,.T.);
#5902=EDGE_CURVE('',#4862,#4853,#4362,.T.);
#5903=EDGE_CURVE('',#4856,#4861,#4363,.T.);
#5904=EDGE_CURVE('',#4855,#4863,#4364,.T.);
#5905=EDGE_CURVE('',#4863,#4864,#2382,.T.);
#5906=EDGE_CURVE('',#4864,#4856,#4365,.T.);
#5907=EDGE_CURVE('',#4865,#4857,#2383,.T.);
#5908=EDGE_CURVE('',#4866,#4865,#2384,.T.);
#5909=EDGE_CURVE('',#4866,#4867,#2385,.T.);
#5910=EDGE_CURVE('',#4867,#4868,#2386,.T.);
#5911=EDGE_CURVE('',#4868,#4869,#2387,.T.);
#5912=EDGE_CURVE('',#4870,#4869,#2388,.T.);
#5913=EDGE_CURVE('',#4870,#4871,#2389,.T.);
#5914=EDGE_CURVE('',#4871,#4872,#2390,.T.);
#5915=EDGE_CURVE('',#4872,#4873,#2391,.T.);
#5916=EDGE_CURVE('',#4873,#4874,#2392,.T.);
#5917=EDGE_CURVE('',#4874,#4875,#2393,.T.);
#5918=EDGE_CURVE('',#4876,#4875,#2394,.T.);
#5919=EDGE_CURVE('',#4876,#4877,#2395,.T.);
#5920=EDGE_CURVE('',#4877,#4878,#2396,.T.);
#5921=EDGE_CURVE('',#4878,#4879,#2397,.T.);
#5922=EDGE_CURVE('',#4880,#4879,#2398,.T.);
#5923=EDGE_CURVE('',#4858,#4880,#2399,.T.);
#5924=EDGE_CURVE('',#4860,#4881,#4366,.T.);
#5925=EDGE_CURVE('',#4881,#4857,#4367,.T.);
#5926=EDGE_CURVE('',#4882,#4863,#4368,.T.);
#5927=EDGE_CURVE('',#4858,#4882,#4369,.T.);
#5928=EDGE_CURVE('',#4883,#4884,#2400,.T.);
#5929=EDGE_CURVE('',#4884,#4885,#2401,.T.);
#5930=EDGE_CURVE('',#4885,#4881,#2402,.T.);
#5931=EDGE_CURVE('',#4883,#4859,#264,.T.);
#5932=EDGE_CURVE('',#4862,#4859,#265,.T.);
#5933=EDGE_CURVE('',#4886,#4887,#2403,.T.);
#5934=EDGE_CURVE('',#4887,#4862,#266,.T.);
#5935=EDGE_CURVE('',#4888,#4861,#267,.T.);
#5936=EDGE_CURVE('',#4888,#4889,#2404,.T.);
#5937=EDGE_CURVE('',#4889,#4886,#2405,.T.);
#5938=EDGE_CURVE('',#4864,#4861,#268,.T.);
#5939=EDGE_CURVE('',#4882,#4890,#2406,.T.);
#5940=EDGE_CURVE('',#4890,#4891,#2407,.T.);
#5941=EDGE_CURVE('',#4891,#4892,#2408,.T.);
#5942=EDGE_CURVE('',#4892,#4864,#269,.T.);
#5943=EDGE_CURVE('',#4893,#4894,#2409,.T.);
#5944=EDGE_CURVE('',#4894,#4879,#4370,.T.);
#5945=EDGE_CURVE('',#4878,#4893,#4371,.T.);
#5946=EDGE_CURVE('',#4895,#4896,#2410,.T.);
#5947=EDGE_CURVE('',#4896,#4877,#4372,.T.);
#5948=EDGE_CURVE('',#4876,#4895,#4373,.T.);
#5949=EDGE_CURVE('',#4897,#4898,#2411,.T.);
#5950=EDGE_CURVE('',#4898,#4875,#4374,.T.);
#5951=EDGE_CURVE('',#4874,#4897,#4375,.T.);
#5952=EDGE_CURVE('',#4899,#4900,#2412,.T.);
#5953=EDGE_CURVE('',#4901,#4899,#4376,.T.);
#5954=EDGE_CURVE('',#4902,#4901,#2413,.T.);
#5955=EDGE_CURVE('',#4903,#4902,#4377,.T.);
#5956=EDGE_CURVE('',#4904,#4903,#2414,.T.);
#5957=EDGE_CURVE('',#4905,#4904,#4378,.T.);
#5958=EDGE_CURVE('',#4906,#4905,#2415,.T.);
#5959=EDGE_CURVE('',#4907,#4906,#4379,.T.);
#5960=EDGE_CURVE('',#4908,#4907,#2416,.T.);
#5961=EDGE_CURVE('',#4909,#4908,#4380,.T.);
#5962=EDGE_CURVE('',#4897,#4909,#2417,.T.);
#5963=EDGE_CURVE('',#4910,#4873,#4381,.T.);
#5964=EDGE_CURVE('',#4911,#4910,#2418,.T.);
#5965=EDGE_CURVE('',#4912,#4911,#4382,.T.);
#5966=EDGE_CURVE('',#4913,#4912,#2419,.T.);
#5967=EDGE_CURVE('',#4914,#4913,#4383,.T.);
#5968=EDGE_CURVE('',#4915,#4914,#2420,.T.);
#5969=EDGE_CURVE('',#4916,#4915,#4384,.T.);
#5970=EDGE_CURVE('',#4917,#4916,#2421,.T.);
#5971=EDGE_CURVE('',#4918,#4917,#4385,.T.);
#5972=EDGE_CURVE('',#4919,#4918,#2422,.T.);
#5973=EDGE_CURVE('',#4920,#4919,#4386,.T.);
#5974=EDGE_CURVE('',#4921,#4920,#2423,.T.);
#5975=EDGE_CURVE('',#4922,#4921,#4387,.T.);
#5976=EDGE_CURVE('',#4923,#4922,#2424,.T.);
#5977=EDGE_CURVE('',#4924,#4923,#4388,.T.);
#5978=EDGE_CURVE('',#4925,#4924,#2425,.T.);
#5979=EDGE_CURVE('',#4926,#4925,#4389,.T.);
#5980=EDGE_CURVE('',#4927,#4926,#2426,.T.);
#5981=EDGE_CURVE('',#4928,#4927,#4390,.T.);
#5982=EDGE_CURVE('',#4929,#4928,#2427,.T.);
#5983=EDGE_CURVE('',#4930,#4929,#4391,.T.);
#5984=EDGE_CURVE('',#4931,#4930,#2428,.T.);
#5985=EDGE_CURVE('',#4872,#4931,#4392,.T.);
#5986=EDGE_CURVE('',#4932,#4871,#4393,.T.);
#5987=EDGE_CURVE('',#4933,#4932,#2429,.T.);
#5988=EDGE_CURVE('',#4900,#4933,#4394,.T.);
#5989=EDGE_CURVE('',#4934,#4873,#4395,.T.);
#5990=EDGE_CURVE('',#4872,#4935,#4396,.T.);
#5991=EDGE_CURVE('',#4935,#4934,#2430,.T.);
#5992=EDGE_CURVE('',#4870,#4936,#4397,.T.);
#5993=EDGE_CURVE('',#4936,#4932,#2431,.T.);
#5994=EDGE_CURVE('',#4868,#4937,#4398,.T.);
#5995=EDGE_CURVE('',#4937,#4938,#2432,.T.);
#5996=EDGE_CURVE('',#4938,#4869,#4399,.T.);
#5997=EDGE_CURVE('',#4866,#4939,#4400,.T.);
#5998=EDGE_CURVE('',#4939,#4940,#2433,.T.);
#5999=EDGE_CURVE('',#4940,#4867,#4401,.T.);
#6000=EDGE_CURVE('',#4885,#4865,#4402,.T.);
#6001=EDGE_CURVE('',#4880,#4890,#4403,.T.);
#6002=EDGE_CURVE('',#4941,#4942,#4404,.T.);
#6003=EDGE_CURVE('',#4942,#4943,#2434,.T.);
#6004=EDGE_CURVE('',#4943,#4944,#4405,.T.);
#6005=EDGE_CURVE('',#4944,#4939,#2435,.T.);
#6006=EDGE_CURVE('',#4884,#4886,#4406,.T.);
#6007=EDGE_CURVE('',#4889,#4891,#4407,.T.);
#6008=EDGE_CURVE('',#4894,#4945,#2436,.T.);
#6009=EDGE_CURVE('',#4945,#4946,#4408,.T.);
#6010=EDGE_CURVE('',#4946,#4947,#2437,.T.);
#6011=EDGE_CURVE('',#4947,#4948,#4409,.T.);
#6012=EDGE_CURVE('',#4948,#4949,#2438,.T.);
#6013=EDGE_CURVE('',#4949,#4950,#4410,.T.);
#6014=EDGE_CURVE('',#4950,#4951,#2439,.T.);
#6015=EDGE_CURVE('',#4951,#4952,#4411,.T.);
#6016=EDGE_CURVE('',#4952,#4941,#2440,.T.);
#6017=EDGE_CURVE('',#4883,#4887,#4412,.T.);
#6018=EDGE_CURVE('',#4888,#4892,#4413,.T.);
#6019=EDGE_CURVE('',#4953,#4954,#2441,.T.);
#6020=EDGE_CURVE('',#4955,#4954,#2442,.T.);
#6021=EDGE_CURVE('',#4955,#4945,#2443,.T.);
#6022=EDGE_CURVE('',#4893,#4956,#2444,.T.);
#6023=EDGE_CURVE('',#4956,#4957,#2445,.T.);
#6024=EDGE_CURVE('',#4957,#4953,#2446,.T.);
#6025=EDGE_CURVE('',#4958,#4896,#2447,.T.);
#6026=EDGE_CURVE('',#4956,#4958,#2448,.T.);
#6027=EDGE_CURVE('',#4959,#4960,#2449,.T.);
#6028=EDGE_CURVE('',#4960,#4961,#2450,.T.);
#6029=EDGE_CURVE('',#4961,#4962,#2451,.T.);
#6030=EDGE_CURVE('',#4962,#4963,#2452,.T.);
#6031=EDGE_CURVE('',#4963,#4964,#2453,.T.);
#6032=EDGE_CURVE('',#4964,#4965,#2454,.T.);
#6033=EDGE_CURVE('',#4965,#4966,#2455,.T.);
#6034=EDGE_CURVE('',#4966,#4967,#2456,.T.);
#6035=EDGE_CURVE('',#4967,#4968,#2457,.T.);
#6036=EDGE_CURVE('',#4968,#4969,#2458,.T.);
#6037=EDGE_CURVE('',#4969,#4970,#2459,.T.);
#6038=EDGE_CURVE('',#4970,#4971,#2460,.T.);
#6039=EDGE_CURVE('',#4971,#4972,#2461,.T.);
#6040=EDGE_CURVE('',#4972,#4973,#2462,.T.);
#6041=EDGE_CURVE('',#4973,#4958,#2463,.T.);
#6042=EDGE_CURVE('',#4895,#4974,#2464,.T.);
#6043=EDGE_CURVE('',#4974,#4975,#2465,.T.);
#6044=EDGE_CURVE('',#4975,#4976,#2466,.T.);
#6045=EDGE_CURVE('',#4976,#4977,#2467,.T.);
#6046=EDGE_CURVE('',#4977,#4978,#2468,.T.);
#6047=EDGE_CURVE('',#4978,#4979,#2469,.T.);
#6048=EDGE_CURVE('',#4979,#4980,#2470,.T.);
#6049=EDGE_CURVE('',#4980,#4981,#2471,.T.);
#6050=EDGE_CURVE('',#4981,#4982,#2472,.T.);
#6051=EDGE_CURVE('',#4982,#4983,#2473,.T.);
#6052=EDGE_CURVE('',#4983,#4984,#2474,.T.);
#6053=EDGE_CURVE('',#4984,#4985,#2475,.T.);
#6054=EDGE_CURVE('',#4985,#4986,#2476,.T.);
#6055=EDGE_CURVE('',#4986,#4987,#2477,.T.);
#6056=EDGE_CURVE('',#4987,#4988,#2478,.T.);
#6057=EDGE_CURVE('',#4988,#4989,#2479,.T.);
#6058=EDGE_CURVE('',#4989,#4990,#2480,.T.);
#6059=EDGE_CURVE('',#4990,#4991,#2481,.T.);
#6060=EDGE_CURVE('',#4991,#4992,#2482,.T.);
#6061=EDGE_CURVE('',#4992,#4993,#2483,.T.);
#6062=EDGE_CURVE('',#4993,#4994,#2484,.T.);
#6063=EDGE_CURVE('',#4994,#4995,#2485,.T.);
#6064=EDGE_CURVE('',#4995,#4959,#2486,.T.);
#6065=EDGE_CURVE('',#4898,#4996,#2487,.T.);
#6066=EDGE_CURVE('',#4996,#4974,#2488,.T.);
#6067=EDGE_CURVE('',#4997,#4998,#2489,.T.);
#6068=EDGE_CURVE('',#4999,#4998,#2490,.T.);
#6069=EDGE_CURVE('',#5000,#4999,#2491,.T.);
#6070=EDGE_CURVE('',#4996,#5000,#2492,.T.);
#6071=EDGE_CURVE('',#4997,#4909,#2493,.T.);
#6072=EDGE_CURVE('',#4933,#5001,#2494,.T.);
#6073=EDGE_CURVE('',#5001,#5002,#4414,.T.);
#6074=EDGE_CURVE('',#5002,#4900,#2495,.T.);
#6075=EDGE_CURVE('',#5003,#5002,#2496,.T.);
#6076=EDGE_CURVE('',#5004,#5003,#2497,.T.);
#6077=EDGE_CURVE('',#5005,#5004,#2498,.T.);
#6078=EDGE_CURVE('',#5006,#5005,#2499,.T.);
#6079=EDGE_CURVE('',#5007,#5006,#2500,.T.);
#6080=EDGE_CURVE('',#5008,#5007,#2501,.T.);
#6081=EDGE_CURVE('',#5009,#5008,#2502,.T.);
#6082=EDGE_CURVE('',#5010,#5009,#2503,.T.);
#6083=EDGE_CURVE('',#5011,#5010,#2504,.T.);
#6084=EDGE_CURVE('',#5012,#5011,#2505,.T.);
#6085=EDGE_CURVE('',#5013,#5012,#2506,.T.);
#6086=EDGE_CURVE('',#5014,#5013,#2507,.T.);
#6087=EDGE_CURVE('',#5015,#5014,#2508,.T.);
#6088=EDGE_CURVE('',#4899,#5015,#2509,.T.);
#6089=EDGE_CURVE('',#5015,#5016,#4415,.T.);
#6090=EDGE_CURVE('',#5016,#4901,#2510,.T.);
#6091=EDGE_CURVE('',#5017,#5016,#2511,.T.);
#6092=EDGE_CURVE('',#4902,#5017,#2512,.T.);
#6093=EDGE_CURVE('',#5018,#5019,#4416,.T.);
#6094=EDGE_CURVE('',#5019,#5020,#4417,.T.);
#6095=EDGE_CURVE('',#5020,#4903,#2513,.T.);
#6096=EDGE_CURVE('',#5017,#5018,#4418,.T.);
#6097=EDGE_CURVE('',#5021,#5020,#2514,.T.);
#6098=EDGE_CURVE('',#5022,#5021,#2515,.T.);
#6099=EDGE_CURVE('',#5023,#5022,#2516,.T.);
#6100=EDGE_CURVE('',#5024,#5023,#2517,.T.);
#6101=EDGE_CURVE('',#5025,#5024,#2518,.T.);
#6102=EDGE_CURVE('',#5026,#5025,#2519,.T.);
#6103=EDGE_CURVE('',#5027,#5026,#2520,.T.);
#6104=EDGE_CURVE('',#5028,#5027,#2521,.T.);
#6105=EDGE_CURVE('',#5029,#5028,#2522,.T.);
#6106=EDGE_CURVE('',#4904,#5029,#2523,.T.);
#6107=EDGE_CURVE('',#5030,#4992,#4419,.T.);
#6108=EDGE_CURVE('',#4992,#5031,#4420,.T.);
#6109=EDGE_CURVE('',#5031,#4905,#2524,.T.);
#6110=EDGE_CURVE('',#5029,#5030,#4421,.T.);
#6111=EDGE_CURVE('',#5032,#5031,#2525,.T.);
#6112=EDGE_CURVE('',#4906,#5032,#2526,.T.);
#6113=EDGE_CURVE('',#5032,#5033,#4422,.T.);
#6114=EDGE_CURVE('',#5033,#4907,#2527,.T.);
#6115=EDGE_CURVE('',#5034,#5033,#2528,.T.);
#6116=EDGE_CURVE('',#5035,#5034,#2529,.T.);
#6117=EDGE_CURVE('',#5036,#5035,#2530,.T.);
#6118=EDGE_CURVE('',#5037,#5036,#2531,.T.);
#6119=EDGE_CURVE('',#5038,#5037,#2532,.T.);
#6120=EDGE_CURVE('',#5039,#5038,#2533,.T.);
#6121=EDGE_CURVE('',#5040,#5039,#2534,.T.);
#6122=EDGE_CURVE('',#5041,#5040,#2535,.T.);
#6123=EDGE_CURVE('',#5042,#5041,#2536,.T.);
#6124=EDGE_CURVE('',#5043,#5042,#2537,.T.);
#6125=EDGE_CURVE('',#5044,#5043,#2538,.T.);
#6126=EDGE_CURVE('',#5045,#5044,#2539,.T.);
#6127=EDGE_CURVE('',#5046,#5045,#2540,.T.);
#6128=EDGE_CURVE('',#4908,#5046,#2541,.T.);
#6129=EDGE_CURVE('',#5046,#4997,#4423,.T.);
#6130=EDGE_CURVE('',#4934,#5047,#4424,.T.);
#6131=EDGE_CURVE('',#5047,#4910,#4425,.T.);
#6132=EDGE_CURVE('',#5048,#5047,#2542,.T.);
#6133=EDGE_CURVE('',#4911,#5048,#2543,.T.);
#6134=EDGE_CURVE('',#4912,#5049,#2544,.T.);
#6135=EDGE_CURVE('',#5049,#5048,#4426,.T.);
#6136=EDGE_CURVE('',#5050,#5051,#270,.T.);
#6137=EDGE_CURVE('',#4913,#5050,#2545,.T.);
#6138=EDGE_CURVE('',#5051,#5049,#2546,.T.);
#6139=EDGE_CURVE('',#5052,#5050,#4427,.T.);
#6140=EDGE_CURVE('',#5052,#4914,#2547,.T.);
#6141=EDGE_CURVE('',#5053,#5052,#271,.T.);
#6142=EDGE_CURVE('',#5053,#5054,#2548,.T.);
#6143=EDGE_CURVE('',#5055,#5054,#272,.T.);
#6144=EDGE_CURVE('',#5055,#4915,#2549,.T.);
#6145=EDGE_CURVE('',#5056,#5055,#4428,.T.);
#6146=EDGE_CURVE('',#5056,#4916,#2550,.T.);
#6147=EDGE_CURVE('',#4917,#5057,#2551,.T.);
#6148=EDGE_CURVE('',#5058,#5056,#273,.T.);
#6149=EDGE_CURVE('',#5057,#5058,#2552,.T.);
#6150=EDGE_CURVE('',#4918,#5059,#2553,.T.);
#6151=EDGE_CURVE('',#5059,#5057,#4429,.T.);
#6152=EDGE_CURVE('',#5060,#5061,#274,.T.);
#6153=EDGE_CURVE('',#4919,#5060,#2554,.T.);
#6154=EDGE_CURVE('',#5061,#5059,#2555,.T.);
#6155=EDGE_CURVE('',#5062,#5060,#4430,.T.);
#6156=EDGE_CURVE('',#5062,#4920,#2556,.T.);
#6157=EDGE_CURVE('',#5063,#5062,#275,.T.);
#6158=EDGE_CURVE('',#5063,#5064,#2557,.T.);
#6159=EDGE_CURVE('',#5065,#5064,#276,.T.);
#6160=EDGE_CURVE('',#5065,#4921,#2558,.T.);
#6161=EDGE_CURVE('',#5066,#5065,#4431,.T.);
#6162=EDGE_CURVE('',#5066,#4922,#2559,.T.);
#6163=EDGE_CURVE('',#4923,#5067,#2560,.T.);
#6164=EDGE_CURVE('',#5068,#5066,#277,.T.);
#6165=EDGE_CURVE('',#5067,#5068,#2561,.T.);
#6166=EDGE_CURVE('',#4924,#5069,#2562,.T.);
#6167=EDGE_CURVE('',#5069,#5067,#4432,.T.);
#6168=EDGE_CURVE('',#5070,#5071,#278,.T.);
#6169=EDGE_CURVE('',#4925,#5070,#2563,.T.);
#6170=EDGE_CURVE('',#5071,#5069,#2564,.T.);
#6171=EDGE_CURVE('',#5072,#5070,#4433,.T.);
#6172=EDGE_CURVE('',#5072,#4926,#2565,.T.);
#6173=EDGE_CURVE('',#5073,#5072,#279,.T.);
#6174=EDGE_CURVE('',#5073,#5074,#2566,.T.);
#6175=EDGE_CURVE('',#5075,#5074,#280,.T.);
#6176=EDGE_CURVE('',#5075,#4927,#2567,.T.);
#6177=EDGE_CURVE('',#5076,#5075,#4434,.T.);
#6178=EDGE_CURVE('',#5076,#4928,#2568,.T.);
#6179=EDGE_CURVE('',#4929,#5077,#2569,.T.);
#6180=EDGE_CURVE('',#5078,#5076,#281,.T.);
#6181=EDGE_CURVE('',#5077,#5078,#2570,.T.);
#6182=EDGE_CURVE('',#4930,#5079,#2571,.T.);
#6183=EDGE_CURVE('',#5079,#5077,#4435,.T.);
#6184=EDGE_CURVE('',#5080,#5079,#2572,.T.);
#6185=EDGE_CURVE('',#4931,#5080,#4436,.T.);
#6186=EDGE_CURVE('',#5080,#4935,#4437,.T.);
#6187=EDGE_CURVE('',#5081,#4936,#2573,.T.);
#6188=EDGE_CURVE('',#5082,#5081,#2574,.T.);
#6189=EDGE_CURVE('',#5083,#5082,#2575,.T.);
#6190=EDGE_CURVE('',#5084,#5083,#2576,.T.);
#6191=EDGE_CURVE('',#5001,#5084,#2577,.T.);
#6192=EDGE_CURVE('',#5085,#5086,#4438,.T.);
#6193=EDGE_CURVE('',#5087,#5085,#2578,.T.);
#6194=EDGE_CURVE('',#5088,#5087,#2579,.T.);
#6195=EDGE_CURVE('',#5089,#5088,#2580,.T.);
#6196=EDGE_CURVE('',#5090,#5089,#4439,.T.);
#6197=EDGE_CURVE('',#5091,#5090,#2581,.T.);
#6198=EDGE_CURVE('',#5092,#5091,#2582,.T.);
#6199=EDGE_CURVE('',#5093,#5092,#2583,.T.);
#6200=EDGE_CURVE('',#5094,#5093,#4440,.T.);
#6201=EDGE_CURVE('',#5095,#5094,#2584,.T.);
#6202=EDGE_CURVE('',#5096,#5095,#2585,.T.);
#6203=EDGE_CURVE('',#5097,#5096,#2586,.T.);
#6204=EDGE_CURVE('',#5098,#5097,#4441,.T.);
#6205=EDGE_CURVE('',#4934,#5098,#2587,.T.);
#6206=EDGE_CURVE('',#5086,#4935,#2588,.T.);
#6207=EDGE_CURVE('',#5099,#5081,#2589,.T.);
#6208=EDGE_CURVE('',#4938,#5099,#2590,.T.);
#6209=EDGE_CURVE('',#5100,#4940,#2591,.T.);
#6210=EDGE_CURVE('',#5101,#5100,#2592,.T.);
#6211=EDGE_CURVE('',#4937,#5101,#2593,.T.);
#6212=EDGE_CURVE('',#5102,#5103,#2594,.T.);
#6213=EDGE_CURVE('',#5103,#5104,#2595,.T.);
#6214=EDGE_CURVE('',#5104,#5105,#2596,.T.);
#6215=EDGE_CURVE('',#5105,#5106,#2597,.T.);
#6216=EDGE_CURVE('',#5106,#5107,#2598,.T.);
#6217=EDGE_CURVE('',#5107,#5108,#2599,.T.);
#6218=EDGE_CURVE('',#5108,#5109,#2600,.T.);
#6219=EDGE_CURVE('',#5109,#5110,#2601,.T.);
#6220=EDGE_CURVE('',#5110,#5018,#2602,.T.);
#6221=EDGE_CURVE('',#5018,#5111,#2603,.T.);
#6222=EDGE_CURVE('',#5111,#5112,#2604,.T.);
#6223=EDGE_CURVE('',#5112,#5113,#2605,.T.);
#6224=EDGE_CURVE('',#5113,#5114,#2606,.T.);
#6225=EDGE_CURVE('',#5114,#5115,#2607,.T.);
#6226=EDGE_CURVE('',#5115,#5116,#2608,.T.);
#6227=EDGE_CURVE('',#5116,#5117,#2609,.T.);
#6228=EDGE_CURVE('',#5117,#5118,#2610,.T.);
#6229=EDGE_CURVE('',#5118,#5119,#2611,.T.);
#6230=EDGE_CURVE('',#5119,#5120,#2612,.T.);
#6231=EDGE_CURVE('',#5120,#5121,#2613,.T.);
#6232=EDGE_CURVE('',#5121,#5122,#2614,.T.);
#6233=EDGE_CURVE('',#5122,#5123,#2615,.T.);
#6234=EDGE_CURVE('',#5123,#5124,#2616,.T.);
#6235=EDGE_CURVE('',#5124,#5125,#2617,.T.);
#6236=EDGE_CURVE('',#5125,#5126,#2618,.T.);
#6237=EDGE_CURVE('',#5126,#5127,#2619,.T.);
#6238=EDGE_CURVE('',#5127,#5099,#2620,.T.);
#6239=EDGE_CURVE('',#5101,#5128,#2621,.T.);
#6240=EDGE_CURVE('',#5128,#5129,#2622,.T.);
#6241=EDGE_CURVE('',#5129,#5130,#2623,.T.);
#6242=EDGE_CURVE('',#5130,#5131,#2624,.T.);
#6243=EDGE_CURVE('',#5131,#5132,#2625,.T.);
#6244=EDGE_CURVE('',#5132,#5133,#2626,.T.);
#6245=EDGE_CURVE('',#5133,#5134,#2627,.T.);
#6246=EDGE_CURVE('',#5134,#5135,#2628,.T.);
#6247=EDGE_CURVE('',#5135,#5136,#2629,.T.);
#6248=EDGE_CURVE('',#5136,#5102,#2630,.T.);
#6249=EDGE_CURVE('',#4944,#5137,#2631,.T.);
#6250=EDGE_CURVE('',#5138,#5137,#2632,.T.);
#6251=EDGE_CURVE('',#5138,#5139,#2633,.T.);
#6252=EDGE_CURVE('',#5139,#5140,#2634,.T.);
#6253=EDGE_CURVE('',#5140,#5100,#2635,.T.);
#6254=EDGE_CURVE('',#5141,#5142,#2636,.T.);
#6255=EDGE_CURVE('',#5142,#5143,#2637,.T.);
#6256=EDGE_CURVE('',#5143,#4943,#2638,.T.);
#6257=EDGE_CURVE('',#4942,#5144,#2639,.T.);
#6258=EDGE_CURVE('',#5144,#5145,#2640,.T.);
#6259=EDGE_CURVE('',#5145,#5146,#2641,.T.);
#6260=EDGE_CURVE('',#5146,#5147,#2642,.T.);
#6261=EDGE_CURVE('',#5147,#5148,#2643,.T.);
#6262=EDGE_CURVE('',#5148,#5149,#2644,.T.);
#6263=EDGE_CURVE('',#5149,#5150,#2645,.T.);
#6264=EDGE_CURVE('',#5150,#5151,#2646,.T.);
#6265=EDGE_CURVE('',#5151,#5152,#2647,.T.);
#6266=EDGE_CURVE('',#5152,#5153,#2648,.T.);
#6267=EDGE_CURVE('',#5153,#5154,#2649,.T.);
#6268=EDGE_CURVE('',#5154,#5141,#2650,.T.);
#6269=EDGE_CURVE('',#4941,#5155,#2651,.T.);
#6270=EDGE_CURVE('',#5155,#5144,#4442,.T.);
#6271=EDGE_CURVE('',#4952,#5156,#2652,.T.);
#6272=EDGE_CURVE('',#5156,#5155,#2653,.T.);
#6273=EDGE_CURVE('',#4951,#5157,#2654,.T.);
#6274=EDGE_CURVE('',#5157,#5158,#4443,.T.);
#6275=EDGE_CURVE('',#5158,#5104,#4444,.T.);
#6276=EDGE_CURVE('',#5104,#5156,#4445,.T.);
#6277=EDGE_CURVE('',#5159,#5160,#2655,.T.);
#6278=EDGE_CURVE('',#5160,#5157,#2656,.T.);
#6279=EDGE_CURVE('',#4950,#5161,#2657,.T.);
#6280=EDGE_CURVE('',#5161,#5162,#2658,.T.);
#6281=EDGE_CURVE('',#5162,#5163,#2659,.T.);
#6282=EDGE_CURVE('',#5163,#5164,#2660,.T.);
#6283=EDGE_CURVE('',#5164,#5165,#2661,.T.);
#6284=EDGE_CURVE('',#5165,#5166,#2662,.T.);
#6285=EDGE_CURVE('',#5166,#5167,#2663,.T.);
#6286=EDGE_CURVE('',#5167,#5159,#2664,.T.);
#6287=EDGE_CURVE('',#4949,#5168,#2665,.T.);
#6288=EDGE_CURVE('',#5168,#4962,#4446,.T.);
#6289=EDGE_CURVE('',#4962,#5169,#4447,.T.);
#6290=EDGE_CURVE('',#5169,#5161,#4448,.T.);
#6291=EDGE_CURVE('',#4948,#5170,#2666,.T.);
#6292=EDGE_CURVE('',#5170,#5168,#2667,.T.);
#6293=EDGE_CURVE('',#4947,#5171,#2668,.T.);
#6294=EDGE_CURVE('',#5171,#5170,#4449,.T.);
#6295=EDGE_CURVE('',#5172,#5173,#2669,.T.);
#6296=EDGE_CURVE('',#5173,#5171,#2670,.T.);
#6297=EDGE_CURVE('',#4946,#5174,#2671,.T.);
#6298=EDGE_CURVE('',#5174,#5175,#2672,.T.);
#6299=EDGE_CURVE('',#5175,#5176,#2673,.T.);
#6300=EDGE_CURVE('',#5176,#5177,#2674,.T.);
#6301=EDGE_CURVE('',#5177,#5178,#2675,.T.);
#6302=EDGE_CURVE('',#5178,#5179,#2676,.T.);
#6303=EDGE_CURVE('',#5179,#5180,#2677,.T.);
#6304=EDGE_CURVE('',#5180,#5181,#2678,.T.);
#6305=EDGE_CURVE('',#5181,#5182,#2679,.T.);
#6306=EDGE_CURVE('',#5182,#5183,#2680,.T.);
#6307=EDGE_CURVE('',#5183,#5184,#2681,.T.);
#6308=EDGE_CURVE('',#5184,#5172,#2682,.T.);
#6309=EDGE_CURVE('',#4955,#5174,#4450,.T.);
#6310=EDGE_CURVE('',#5143,#5137,#4451,.T.);
#6311=EDGE_CURVE('',#5185,#4953,#2683,.T.);
#6312=EDGE_CURVE('',#5186,#5185,#2684,.T.);
#6313=EDGE_CURVE('',#4954,#5186,#2685,.T.);
#6314=EDGE_CURVE('',#4973,#4957,#2686,.T.);
#6315=EDGE_CURVE('',#5185,#4972,#2687,.T.);
#6316=EDGE_CURVE('',#4960,#5187,#2688,.T.);
#6317=EDGE_CURVE('',#5187,#5169,#2689,.T.);
#6318=EDGE_CURVE('',#5169,#4961,#2690,.T.);
#6319=EDGE_CURVE('',#5188,#5189,#2691,.T.);
#6320=EDGE_CURVE('',#5187,#5188,#2692,.T.);
#6321=EDGE_CURVE('',#5190,#4959,#4452,.T.);
#6322=EDGE_CURVE('',#5189,#5190,#2693,.T.);
#6323=EDGE_CURVE('',#5191,#5190,#2694,.T.);
#6324=EDGE_CURVE('',#4995,#5191,#4453,.T.);
#6325=EDGE_CURVE('',#5192,#5191,#2695,.T.);
#6326=EDGE_CURVE('',#4994,#5193,#2696,.T.);
#6327=EDGE_CURVE('',#5193,#5194,#2697,.T.);
#6328=EDGE_CURVE('',#5194,#5192,#2698,.T.);
#6329=EDGE_CURVE('',#5193,#5030,#2699,.T.);
#6330=EDGE_CURVE('',#5030,#4993,#2700,.T.);
#6331=EDGE_CURVE('',#4991,#5195,#2701,.T.);
#6332=EDGE_CURVE('',#5195,#5196,#2702,.T.);
#6333=EDGE_CURVE('',#5196,#5034,#2703,.T.);
#6334=EDGE_CURVE('',#5197,#5195,#2704,.T.);
#6335=EDGE_CURVE('',#4990,#5197,#2705,.T.);
#6336=EDGE_CURVE('',#5198,#4988,#2706,.T.);
#6337=EDGE_CURVE('',#5199,#5198,#2707,.T.);
#6338=EDGE_CURVE('',#4989,#5199,#2708,.T.);
#6339=EDGE_CURVE('',#5200,#4987,#2709,.T.);
#6340=EDGE_CURVE('',#5198,#5200,#2710,.T.);
#6341=EDGE_CURVE('',#5200,#5201,#2711,.T.);
#6342=EDGE_CURVE('',#5201,#4986,#2712,.T.);
#6343=EDGE_CURVE('',#5202,#5203,#2713,.T.);
#6344=EDGE_CURVE('',#5203,#4985,#2714,.T.);
#6345=EDGE_CURVE('',#4984,#5202,#2715,.T.);
#6346=EDGE_CURVE('',#5035,#5204,#2716,.T.);
#6347=EDGE_CURVE('',#5204,#5202,#2717,.T.);
#6348=EDGE_CURVE('',#4983,#5205,#2718,.T.);
#6349=EDGE_CURVE('',#5205,#5036,#2719,.T.);
#6350=EDGE_CURVE('',#5206,#4982,#2720,.T.);
#6351=EDGE_CURVE('',#5206,#4983,#2721,.T.);
#6352=EDGE_CURVE('',#4981,#5040,#2722,.T.);
#6353=EDGE_CURVE('',#5039,#5207,#2723,.T.);
#6354=EDGE_CURVE('',#5207,#4982,#2724,.T.);
#6355=EDGE_CURVE('',#5041,#4980,#2725,.T.);
#6356=EDGE_CURVE('',#4979,#5042,#2726,.T.);
#6357=EDGE_CURVE('',#5043,#4978,#2727,.T.);
#6358=EDGE_CURVE('',#4977,#5208,#2728,.T.);
#6359=EDGE_CURVE('',#5208,#5044,#2729,.T.);
#6360=EDGE_CURVE('',#5209,#4976,#2730,.T.);
#6361=EDGE_CURVE('',#5209,#4977,#2731,.T.);
#6362=EDGE_CURVE('',#4975,#5000,#2732,.T.);
#6363=EDGE_CURVE('',#4999,#5210,#2733,.T.);
#6364=EDGE_CURVE('',#5210,#4976,#2734,.T.);
#6365=EDGE_CURVE('',#4971,#5211,#2735,.T.);
#6366=EDGE_CURVE('',#4972,#5211,#2736,.T.);
#6367=EDGE_CURVE('',#5177,#4970,#2737,.T.);
#6368=EDGE_CURVE('',#5212,#5176,#2738,.T.);
#6369=EDGE_CURVE('',#4971,#5212,#2739,.T.);
#6370=EDGE_CURVE('',#4969,#5178,#2740,.T.);
#6371=EDGE_CURVE('',#5179,#4968,#2741,.T.);
#6372=EDGE_CURVE('',#4967,#5180,#2742,.T.);
#6373=EDGE_CURVE('',#5213,#4966,#2743,.T.);
#6374=EDGE_CURVE('',#5181,#5213,#2744,.T.);
#6375=EDGE_CURVE('',#4965,#5214,#2745,.T.);
#6376=EDGE_CURVE('',#4966,#5214,#2746,.T.);
#6377=EDGE_CURVE('',#5172,#4964,#2747,.T.);
#6378=EDGE_CURVE('',#5215,#5184,#2748,.T.);
#6379=EDGE_CURVE('',#4965,#5215,#2749,.T.);
#6380=EDGE_CURVE('',#4963,#5173,#2750,.T.);
#6381=EDGE_CURVE('',#5216,#5210,#2751,.T.);
#6382=EDGE_CURVE('',#4998,#5216,#2752,.T.);
#6383=EDGE_CURVE('',#5217,#5019,#2753,.T.);
#6384=EDGE_CURVE('',#5218,#5217,#2754,.T.);
#6385=EDGE_CURVE('',#5219,#5218,#2755,.T.);
#6386=EDGE_CURVE('',#5021,#5219,#2756,.T.);
#6387=EDGE_CURVE('',#5220,#5010,#2757,.T.);
#6388=EDGE_CURVE('',#5221,#5220,#2758,.T.);
#6389=EDGE_CURVE('',#5222,#5221,#2759,.T.);
#6390=EDGE_CURVE('',#5011,#5222,#2760,.T.);
#6391=EDGE_CURVE('',#5223,#5084,#2761,.T.);
#6392=EDGE_CURVE('',#5224,#5223,#2762,.T.);
#6393=EDGE_CURVE('',#5225,#5224,#2763,.T.);
#6394=EDGE_CURVE('',#5003,#5225,#2764,.T.);
#6395=EDGE_CURVE('',#5226,#5028,#2765,.T.);
#6396=EDGE_CURVE('',#5227,#5226,#2766,.T.);
#6397=EDGE_CURVE('',#5228,#5227,#2767,.T.);
#6398=EDGE_CURVE('',#5030,#5228,#2768,.T.);
#6399=EDGE_CURVE('',#5229,#5037,#2769,.T.);
#6400=EDGE_CURVE('',#5230,#5229,#2770,.T.);
#6401=EDGE_CURVE('',#5231,#5230,#2771,.T.);
#6402=EDGE_CURVE('',#5038,#5231,#2772,.T.);
#6403=EDGE_CURVE('',#5232,#5045,#2773,.T.);
#6404=EDGE_CURVE('',#5233,#5232,#2774,.T.);
#6405=EDGE_CURVE('',#5216,#5233,#2775,.T.);
#6406=EDGE_CURVE('',#5225,#5234,#2776,.T.);
#6407=EDGE_CURVE('',#5234,#5004,#2777,.T.);
#6408=EDGE_CURVE('',#5006,#5123,#2778,.T.);
#6409=EDGE_CURVE('',#5124,#5005,#2779,.T.);
#6410=EDGE_CURVE('',#5122,#5007,#2780,.T.);
#6411=EDGE_CURVE('',#5008,#5121,#2781,.T.);
#6412=EDGE_CURVE('',#5235,#5220,#2782,.T.);
#6413=EDGE_CURVE('',#5009,#5235,#2783,.T.);
#6414=EDGE_CURVE('',#5222,#5236,#2784,.T.);
#6415=EDGE_CURVE('',#5236,#5012,#2785,.T.);
#6416=EDGE_CURVE('',#5014,#5237,#2786,.T.);
#6417=EDGE_CURVE('',#5238,#5013,#2787,.T.);
#6418=EDGE_CURVE('',#5237,#5238,#2788,.T.);
#6419=EDGE_CURVE('',#5237,#5239,#2789,.T.);
#6420=EDGE_CURVE('',#5239,#5111,#2790,.T.);
#6421=EDGE_CURVE('',#5019,#5110,#2791,.T.);
#6422=EDGE_CURVE('',#5219,#5240,#2792,.T.);
#6423=EDGE_CURVE('',#5240,#5022,#2793,.T.);
#6424=EDGE_CURVE('',#5024,#5241,#2794,.T.);
#6425=EDGE_CURVE('',#5242,#5023,#2795,.T.);
#6426=EDGE_CURVE('',#5241,#5242,#2796,.T.);
#6427=EDGE_CURVE('',#5243,#5025,#2797,.T.);
#6428=EDGE_CURVE('',#5241,#5243,#2798,.T.);
#6429=EDGE_CURVE('',#5026,#5244,#2799,.T.);
#6430=EDGE_CURVE('',#5244,#5243,#2800,.T.);
#6431=EDGE_CURVE('',#5245,#5226,#2801,.T.);
#6432=EDGE_CURVE('',#5027,#5245,#2802,.T.);
#6433=EDGE_CURVE('',#5204,#5196,#2803,.T.);
#6434=EDGE_CURVE('',#5205,#5229,#2804,.T.);
#6435=EDGE_CURVE('',#5231,#5207,#2805,.T.);
#6436=EDGE_CURVE('',#5208,#5232,#2806,.T.);
#6437=EDGE_CURVE('',#5098,#5048,#4454,.T.);
#6438=EDGE_CURVE('',#5097,#5049,#4455,.T.);
#6439=EDGE_CURVE('',#5096,#5051,#4456,.T.);
#6440=EDGE_CURVE('',#5053,#5096,#4457,.T.);
#6441=EDGE_CURVE('',#5095,#5054,#4458,.T.);
#6442=EDGE_CURVE('',#5094,#5057,#4459,.T.);
#6443=EDGE_CURVE('',#5058,#5095,#4460,.T.);
#6444=EDGE_CURVE('',#5093,#5059,#4461,.T.);
#6445=EDGE_CURVE('',#5092,#5061,#4462,.T.);
#6446=EDGE_CURVE('',#5063,#5092,#4463,.T.);
#6447=EDGE_CURVE('',#5091,#5064,#4464,.T.);
#6448=EDGE_CURVE('',#5090,#5067,#4465,.T.);
#6449=EDGE_CURVE('',#5068,#5091,#4466,.T.);
#6450=EDGE_CURVE('',#5089,#5069,#4467,.T.);
#6451=EDGE_CURVE('',#5088,#5071,#4468,.T.);
#6452=EDGE_CURVE('',#5073,#5088,#4469,.T.);
#6453=EDGE_CURVE('',#5087,#5074,#4470,.T.);
#6454=EDGE_CURVE('',#5085,#5077,#4471,.T.);
#6455=EDGE_CURVE('',#5078,#5087,#4472,.T.);
#6456=EDGE_CURVE('',#5086,#5079,#4473,.T.);
#6457=EDGE_CURVE('',#5082,#5127,#2807,.T.);
#6458=EDGE_CURVE('',#5126,#5246,#2808,.T.);
#6459=EDGE_CURVE('',#5246,#5083,#2809,.T.);
#6460=EDGE_CURVE('',#5246,#5223,#2810,.T.);
#6461=EDGE_CURVE('',#5140,#5128,#2811,.T.);
#6462=EDGE_CURVE('',#5145,#5103,#2812,.T.);
#6463=EDGE_CURVE('',#5102,#5146,#2813,.T.);
#6464=EDGE_CURVE('',#5247,#5136,#2814,.T.);
#6465=EDGE_CURVE('',#5147,#5247,#2815,.T.);
#6466=EDGE_CURVE('',#5135,#5248,#2816,.T.);
#6467=EDGE_CURVE('',#5136,#5248,#2817,.T.);
#6468=EDGE_CURVE('',#5151,#5134,#2818,.T.);
#6469=EDGE_CURVE('',#5249,#5150,#2819,.T.);
#6470=EDGE_CURVE('',#5135,#5249,#2820,.T.);
#6471=EDGE_CURVE('',#5133,#5152,#2821,.T.);
#6472=EDGE_CURVE('',#5153,#5132,#2822,.T.);
#6473=EDGE_CURVE('',#5131,#5154,#2823,.T.);
#6474=EDGE_CURVE('',#5250,#5130,#2824,.T.);
#6475=EDGE_CURVE('',#5141,#5250,#2825,.T.);
#6476=EDGE_CURVE('',#5129,#5251,#2826,.T.);
#6477=EDGE_CURVE('',#5130,#5251,#2827,.T.);
#6478=EDGE_CURVE('',#5252,#5139,#2828,.T.);
#6479=EDGE_CURVE('',#5129,#5252,#2829,.T.);
#6480=EDGE_CURVE('',#5125,#5253,#2830,.T.);
#6481=EDGE_CURVE('',#5253,#5126,#2831,.T.);
#6482=EDGE_CURVE('',#5234,#5125,#2832,.T.);
#6483=EDGE_CURVE('',#5120,#5235,#2833,.T.);
#6484=EDGE_CURVE('',#5119,#5254,#2834,.T.);
#6485=EDGE_CURVE('',#5254,#5120,#2835,.T.);
#6486=EDGE_CURVE('',#5236,#5119,#2836,.T.);
#6487=EDGE_CURVE('',#5118,#5255,#2837,.T.);
#6488=EDGE_CURVE('',#5255,#5238,#2838,.T.);
#6489=EDGE_CURVE('',#5256,#5255,#2839,.T.);
#6490=EDGE_CURVE('',#5117,#5256,#2840,.T.);
#6491=EDGE_CURVE('',#5257,#5115,#2841,.T.);
#6492=EDGE_CURVE('',#5258,#5257,#2842,.T.);
#6493=EDGE_CURVE('',#5116,#5258,#2843,.T.);
#6494=EDGE_CURVE('',#5259,#5114,#2844,.T.);
#6495=EDGE_CURVE('',#5257,#5259,#2845,.T.);
#6496=EDGE_CURVE('',#5259,#5260,#2846,.T.);
#6497=EDGE_CURVE('',#5260,#5113,#2847,.T.);
#6498=EDGE_CURVE('',#5239,#5261,#2848,.T.);
#6499=EDGE_CURVE('',#5261,#5112,#2849,.T.);
#6500=EDGE_CURVE('',#5262,#5109,#2850,.T.);
#6501=EDGE_CURVE('',#5019,#5262,#2851,.T.);
#6502=EDGE_CURVE('',#5108,#5263,#4474,.T.);
#6503=EDGE_CURVE('',#5263,#5264,#2852,.T.);
#6504=EDGE_CURVE('',#5264,#5265,#2853,.T.);
#6505=EDGE_CURVE('',#5265,#5262,#2854,.T.);
#6506=EDGE_CURVE('',#5107,#5266,#4475,.T.);
#6507=EDGE_CURVE('',#5266,#5263,#2855,.T.);
#6508=EDGE_CURVE('',#5267,#5106,#2856,.T.);
#6509=EDGE_CURVE('',#5268,#5267,#2857,.T.);
#6510=EDGE_CURVE('',#5269,#5268,#2858,.T.);
#6511=EDGE_CURVE('',#5266,#5269,#2859,.T.);
#6512=EDGE_CURVE('',#5105,#5158,#2860,.T.);
#6513=EDGE_CURVE('',#5158,#5267,#2861,.T.);
#6514=EDGE_CURVE('',#5270,#5138,#2862,.T.);
#6515=EDGE_CURVE('',#5252,#5270,#2863,.T.);
#6516=EDGE_CURVE('',#5271,#5158,#2864,.T.);
#6517=EDGE_CURVE('',#5160,#5272,#2865,.T.);
#6518=EDGE_CURVE('',#5272,#5273,#2866,.T.);
#6519=EDGE_CURVE('',#5273,#5271,#2867,.T.);
#6520=EDGE_CURVE('',#5274,#5275,#2868,.T.);
#6521=EDGE_CURVE('',#5275,#5149,#2869,.T.);
#6522=EDGE_CURVE('',#5148,#5276,#2870,.T.);
#6523=EDGE_CURVE('',#5276,#5274,#2871,.T.);
#6524=EDGE_CURVE('',#5142,#5277,#2872,.T.);
#6525=EDGE_CURVE('',#5277,#5278,#2873,.T.);
#6526=EDGE_CURVE('',#5278,#5270,#2874,.T.);
#6527=EDGE_CURVE('',#5279,#5162,#2875,.T.);
#6528=EDGE_CURVE('',#5169,#5280,#2876,.T.);
#6529=EDGE_CURVE('',#5280,#5281,#2877,.T.);
#6530=EDGE_CURVE('',#5281,#5279,#2878,.T.);
#6531=EDGE_CURVE('',#5282,#5283,#2879,.T.);
#6532=EDGE_CURVE('',#5283,#5183,#2880,.T.);
#6533=EDGE_CURVE('',#5182,#5284,#2881,.T.);
#6534=EDGE_CURVE('',#5284,#5282,#2882,.T.);
#6535=EDGE_CURVE('',#5285,#5175,#2883,.T.);
#6536=EDGE_CURVE('',#5186,#5286,#2884,.T.);
#6537=EDGE_CURVE('',#5286,#5285,#2885,.T.);
#6538=EDGE_CURVE('',#5277,#5250,#2886,.T.);
#6539=EDGE_CURVE('',#5249,#5275,#2887,.T.);
#6540=EDGE_CURVE('',#5276,#5247,#2888,.T.);
#6541=EDGE_CURVE('',#5287,#5159,#2889,.T.);
#6542=EDGE_CURVE('',#5272,#5287,#2890,.T.);
#6543=EDGE_CURVE('',#5166,#5288,#2891,.T.);
#6544=EDGE_CURVE('',#5288,#5289,#2892,.T.);
#6545=EDGE_CURVE('',#5289,#5167,#2893,.T.);
#6546=EDGE_CURVE('',#5290,#5165,#2894,.T.);
#6547=EDGE_CURVE('',#5288,#5290,#2895,.T.);
#6548=EDGE_CURVE('',#5164,#5291,#2896,.T.);
#6549=EDGE_CURVE('',#5291,#5290,#2897,.T.);
#6550=EDGE_CURVE('',#5292,#5279,#2898,.T.);
#6551=EDGE_CURVE('',#5163,#5292,#2899,.T.);
#6552=EDGE_CURVE('',#5215,#5283,#2900,.T.);
#6553=EDGE_CURVE('',#5284,#5213,#2901,.T.);
#6554=EDGE_CURVE('',#5212,#5285,#2902,.T.);
#6555=EDGE_CURVE('',#5286,#5211,#2903,.T.);
#6556=EDGE_CURVE('',#5280,#5188,#2904,.T.);
#6557=EDGE_CURVE('',#5293,#5189,#2905,.T.);
#6558=EDGE_CURVE('',#5281,#5293,#2906,.T.);
#6559=EDGE_CURVE('',#5294,#5264,#2907,.T.);
#6560=EDGE_CURVE('',#5269,#5295,#2908,.T.);
#6561=EDGE_CURVE('',#5295,#5289,#2909,.T.);
#6562=EDGE_CURVE('',#5291,#5296,#2910,.T.);
#6563=EDGE_CURVE('',#5296,#5189,#2911,.T.);
#6564=EDGE_CURVE('',#5192,#5297,#2912,.T.);
#6565=EDGE_CURVE('',#5297,#5244,#2913,.T.);
#6566=EDGE_CURVE('',#5242,#5294,#2914,.T.);
#6567=EDGE_CURVE('',#5227,#5298,#2915,.T.);
#6568=EDGE_CURVE('',#5298,#5192,#2916,.T.);
#6569=EDGE_CURVE('',#5194,#5228,#2917,.T.);
#6570=EDGE_CURVE('',#5197,#5203,#2918,.T.);
#6571=EDGE_CURVE('',#5201,#5199,#2919,.T.);
#6572=EDGE_CURVE('',#5299,#5300,#2920,.T.);
#6573=EDGE_CURVE('',#5301,#5299,#2921,.T.);
#6574=EDGE_CURVE('',#5302,#5301,#2922,.T.);
#6575=EDGE_CURVE('',#5300,#5302,#2923,.T.);
#6576=EDGE_CURVE('',#5206,#5230,#2924,.T.);
#6577=EDGE_CURVE('',#5209,#5233,#2925,.T.);
#6578=EDGE_CURVE('',#5282,#5214,#2926,.T.);
#6579=EDGE_CURVE('',#5265,#5217,#2927,.T.);
#6580=EDGE_CURVE('',#5264,#5303,#2928,.T.);
#6581=EDGE_CURVE('',#5303,#5218,#2929,.T.);
#6582=EDGE_CURVE('',#5303,#5294,#2930,.T.);
#6583=EDGE_CURVE('',#5294,#5240,#2931,.T.);
#6584=EDGE_CURVE('',#5254,#5221,#2932,.T.);
#6585=EDGE_CURVE('',#5253,#5224,#2933,.T.);
#6586=EDGE_CURVE('',#5245,#5297,#2934,.T.);
#6587=EDGE_CURVE('',#5297,#5298,#2935,.T.);
#6588=EDGE_CURVE('',#5256,#5261,#2936,.T.);
#6589=EDGE_CURVE('',#5053,#5051,#282,.T.);
#6590=EDGE_CURVE('',#5058,#5054,#283,.T.);
#6591=EDGE_CURVE('',#5063,#5061,#284,.T.);
#6592=EDGE_CURVE('',#5068,#5064,#285,.T.);
#6593=EDGE_CURVE('',#5073,#5071,#286,.T.);
#6594=EDGE_CURVE('',#5078,#5074,#287,.T.);
#6595=EDGE_CURVE('',#5274,#5248,#2937,.T.);
#6596=EDGE_CURVE('',#5278,#5251,#2938,.T.);
#6597=EDGE_CURVE('',#5260,#5258,#2939,.T.);
#6598=EDGE_CURVE('',#5304,#5305,#2940,.T.);
#6599=EDGE_CURVE('',#5306,#5304,#2941,.T.);
#6600=EDGE_CURVE('',#5307,#5306,#2942,.T.);
#6601=EDGE_CURVE('',#5305,#5307,#2943,.T.);
#6602=EDGE_CURVE('',#5268,#5271,#2944,.T.);
#6603=EDGE_CURVE('',#5308,#5273,#2945,.T.);
#6604=EDGE_CURVE('',#5269,#5308,#2946,.T.);
#6605=EDGE_CURVE('',#5308,#5295,#2947,.T.);
#6606=EDGE_CURVE('',#5295,#5287,#2948,.T.);
#6607=EDGE_CURVE('',#5296,#5293,#2949,.T.);
#6608=EDGE_CURVE('',#5292,#5296,#2950,.T.);
#6609=EDGE_CURVE('',#5309,#5310,#2951,.T.);
#6610=EDGE_CURVE('',#5310,#5300,#2952,.T.);
#6611=EDGE_CURVE('',#5302,#5309,#2953,.T.);
#6612=EDGE_CURVE('',#5310,#5311,#2954,.T.);
#6613=EDGE_CURVE('',#5311,#5299,#2955,.T.);
#6614=EDGE_CURVE('',#5311,#5312,#2956,.T.);
#6615=EDGE_CURVE('',#5312,#5301,#2957,.T.);
#6616=EDGE_CURVE('',#5312,#5309,#2958,.T.);
#6617=EDGE_CURVE('',#5313,#5314,#2959,.T.);
#6618=EDGE_CURVE('',#5314,#5305,#2960,.T.);
#6619=EDGE_CURVE('',#5307,#5313,#2961,.T.);
#6620=EDGE_CURVE('',#5314,#5315,#2962,.T.);
#6621=EDGE_CURVE('',#5315,#5304,#2963,.T.);
#6622=EDGE_CURVE('',#5315,#5316,#2964,.T.);
#6623=EDGE_CURVE('',#5316,#5306,#2965,.T.);
#6624=EDGE_CURVE('',#5316,#5313,#2966,.T.);
#6625=EDGE_CURVE('',#5317,#5317,#4476,.T.);
#6626=EDGE_CURVE('',#5317,#5318,#2967,.T.);
#6627=EDGE_CURVE('',#5318,#5318,#4477,.T.);
#6628=EDGE_CURVE('',#5319,#5319,#4478,.T.);
#6629=EDGE_CURVE('',#5319,#5320,#2968,.T.);
#6630=EDGE_CURVE('',#5320,#5320,#4479,.T.);
#6631=EDGE_CURVE('',#5321,#5321,#4480,.T.);
#6632=EDGE_CURVE('',#5321,#5322,#2969,.T.);
#6633=EDGE_CURVE('',#5322,#5322,#4481,.T.);
#6634=EDGE_CURVE('',#5323,#5323,#4482,.T.);
#6635=EDGE_CURVE('',#5323,#5324,#2970,.T.);
#6636=EDGE_CURVE('',#5324,#5324,#4483,.T.);
#6637=EDGE_CURVE('',#5325,#5325,#4484,.T.);
#6638=EDGE_CURVE('',#5325,#5326,#2971,.T.);
#6639=EDGE_CURVE('',#5326,#5326,#4485,.T.);
#6640=EDGE_CURVE('',#5327,#5327,#4486,.T.);
#6641=EDGE_CURVE('',#5327,#5328,#2972,.T.);
#6642=EDGE_CURVE('',#5328,#5328,#4487,.T.);
#6643=EDGE_CURVE('',#5329,#5329,#4488,.T.);
#6644=EDGE_CURVE('',#5329,#5330,#2973,.T.);
#6645=EDGE_CURVE('',#5330,#5330,#4489,.T.);
#6646=EDGE_CURVE('',#5331,#5331,#4490,.T.);
#6647=EDGE_CURVE('',#5331,#5332,#2974,.T.);
#6648=EDGE_CURVE('',#5332,#5332,#4491,.T.);
#6649=EDGE_CURVE('',#5333,#5333,#4492,.T.);
#6650=EDGE_CURVE('',#5333,#5334,#2975,.T.);
#6651=EDGE_CURVE('',#5334,#5334,#4493,.T.);
#6652=EDGE_CURVE('',#5335,#5335,#4494,.T.);
#6653=EDGE_CURVE('',#5335,#5336,#2976,.T.);
#6654=EDGE_CURVE('',#5336,#5336,#4495,.T.);
#6655=EDGE_CURVE('',#5337,#5337,#4496,.T.);
#6656=EDGE_CURVE('',#5337,#5338,#2977,.T.);
#6657=EDGE_CURVE('',#5338,#5338,#4497,.T.);
#6658=EDGE_CURVE('',#5339,#5339,#4498,.T.);
#6659=EDGE_CURVE('',#5339,#5340,#2978,.T.);
#6660=EDGE_CURVE('',#5340,#5340,#4499,.T.);
#6661=EDGE_CURVE('',#5341,#5341,#4500,.T.);
#6662=EDGE_CURVE('',#5341,#5342,#2979,.T.);
#6663=EDGE_CURVE('',#5342,#5342,#4501,.T.);
#6664=EDGE_CURVE('',#5343,#5343,#4502,.T.);
#6665=EDGE_CURVE('',#5343,#5344,#2980,.T.);
#6666=EDGE_CURVE('',#5344,#5344,#4503,.T.);
#6667=EDGE_CURVE('',#5345,#5345,#4504,.T.);
#6668=EDGE_CURVE('',#5345,#5346,#2981,.T.);
#6669=EDGE_CURVE('',#5346,#5346,#4505,.T.);
#6670=EDGE_CURVE('',#5347,#5347,#4506,.T.);
#6671=EDGE_CURVE('',#5347,#5348,#2982,.T.);
#6672=EDGE_CURVE('',#5348,#5348,#4507,.T.);
#6673=EDGE_CURVE('',#5349,#5349,#4508,.T.);
#6674=EDGE_CURVE('',#5349,#5350,#2983,.T.);
#6675=EDGE_CURVE('',#5350,#5350,#4509,.T.);
#6676=EDGE_CURVE('',#5351,#5351,#4510,.T.);
#6677=EDGE_CURVE('',#5351,#5352,#2984,.T.);
#6678=EDGE_CURVE('',#5352,#5352,#4511,.T.);
#6679=EDGE_CURVE('',#5353,#5353,#4512,.T.);
#6680=EDGE_CURVE('',#5353,#5354,#2985,.T.);
#6681=EDGE_CURVE('',#5354,#5354,#4513,.T.);
#6682=EDGE_CURVE('',#5355,#5355,#4514,.T.);
#6683=EDGE_CURVE('',#5355,#5356,#2986,.T.);
#6684=EDGE_CURVE('',#5356,#5356,#4515,.T.);
#6685=EDGE_CURVE('',#5357,#5357,#4516,.T.);
#6686=EDGE_CURVE('',#5357,#5358,#2987,.T.);
#6687=EDGE_CURVE('',#5358,#5358,#4517,.T.);
#6688=EDGE_CURVE('',#5359,#5359,#4518,.T.);
#6689=EDGE_CURVE('',#5359,#5360,#2988,.T.);
#6690=EDGE_CURVE('',#5360,#5360,#4519,.T.);
#6691=EDGE_CURVE('',#5361,#5361,#4520,.T.);
#6692=EDGE_CURVE('',#5361,#5362,#2989,.T.);
#6693=EDGE_CURVE('',#5362,#5362,#4521,.T.);
#6694=EDGE_CURVE('',#5363,#5363,#4522,.T.);
#6695=EDGE_CURVE('',#5363,#5364,#2990,.T.);
#6696=EDGE_CURVE('',#5364,#5364,#4523,.T.);
#6697=EDGE_CURVE('',#5365,#5365,#4524,.T.);
#6698=EDGE_CURVE('',#5365,#5366,#2991,.T.);
#6699=EDGE_CURVE('',#5366,#5366,#4525,.T.);
#6700=EDGE_CURVE('',#5326,#5367,#2992,.T.);
#6701=EDGE_CURVE('',#5367,#5367,#4526,.T.);
#6702=EDGE_CURVE('',#5328,#5368,#2993,.T.);
#6703=EDGE_CURVE('',#5368,#5368,#4527,.T.);
#6704=EDGE_CURVE('',#5330,#5369,#2994,.T.);
#6705=EDGE_CURVE('',#5369,#5369,#4528,.T.);
#6706=EDGE_CURVE('',#5332,#5370,#2995,.T.);
#6707=EDGE_CURVE('',#5370,#5370,#4529,.T.);
#6708=EDGE_CURVE('',#5342,#5371,#2996,.T.);
#6709=EDGE_CURVE('',#5371,#5371,#4530,.T.);
#6710=EDGE_CURVE('',#5344,#5372,#2997,.T.);
#6711=EDGE_CURVE('',#5372,#5372,#4531,.T.);
#6712=EDGE_CURVE('',#5346,#5373,#2998,.T.);
#6713=EDGE_CURVE('',#5373,#5373,#4532,.T.);
#6714=EDGE_CURVE('',#5348,#5374,#2999,.T.);
#6715=EDGE_CURVE('',#5374,#5374,#4533,.T.);
#6716=EDGE_CURVE('',#5366,#5375,#3000,.T.);
#6717=EDGE_CURVE('',#5375,#5375,#4534,.T.);
#6718=EDGE_CURVE('',#5376,#5376,#4535,.T.);
#6719=EDGE_CURVE('',#5376,#5377,#3001,.T.);
#6720=EDGE_CURVE('',#5377,#5377,#4536,.T.);
#6721=EDGE_CURVE('',#5378,#5378,#4537,.T.);
#6722=EDGE_CURVE('',#5378,#5379,#3002,.T.);
#6723=EDGE_CURVE('',#5379,#5379,#4538,.T.);
#6724=EDGE_CURVE('',#5380,#5380,#4539,.T.);
#6725=EDGE_CURVE('',#5380,#5381,#3003,.T.);
#6726=EDGE_CURVE('',#5381,#5381,#4540,.T.);
#6727=EDGE_CURVE('',#5382,#5382,#4541,.T.);
#6728=EDGE_CURVE('',#5382,#5383,#3004,.T.);
#6729=EDGE_CURVE('',#5383,#5383,#4542,.T.);
#6730=EDGE_CURVE('',#5384,#5384,#4543,.T.);
#6731=EDGE_CURVE('',#5384,#5385,#3005,.T.);
#6732=EDGE_CURVE('',#5385,#5385,#4544,.T.);
#6733=EDGE_CURVE('',#5386,#5386,#4545,.T.);
#6734=EDGE_CURVE('',#5386,#5387,#3006,.T.);
#6735=EDGE_CURVE('',#5387,#5387,#4546,.T.);
#6736=EDGE_CURVE('',#5388,#5388,#4547,.T.);
#6737=EDGE_CURVE('',#5388,#5389,#3007,.T.);
#6738=EDGE_CURVE('',#5389,#5389,#4548,.T.);
#6739=EDGE_CURVE('',#5390,#5390,#4549,.T.);
#6740=EDGE_CURVE('',#5390,#5391,#3008,.T.);
#6741=EDGE_CURVE('',#5391,#5391,#4550,.T.);
#6742=EDGE_CURVE('',#5392,#5393,#3009,.T.);
#6743=EDGE_CURVE('',#5394,#5392,#3010,.T.);
#6744=EDGE_CURVE('',#5395,#5394,#4551,.T.);
#6745=EDGE_CURVE('',#5396,#5395,#3011,.T.);
#6746=EDGE_CURVE('',#5397,#5396,#4552,.T.);
#6747=EDGE_CURVE('',#5393,#5397,#3012,.T.);
#6748=EDGE_CURVE('',#5398,#5393,#4553,.T.);
#6749=EDGE_CURVE('',#5399,#5397,#288,.T.);
#6750=EDGE_CURVE('',#5399,#5400,#203,.T.);
#6751=EDGE_CURVE('',#5398,#5400,#3013,.T.);
#6752=EDGE_CURVE('',#5398,#5401,#3014,.T.);
#6753=EDGE_CURVE('',#5402,#5401,#3015,.T.);
#6754=EDGE_CURVE('',#5403,#5402,#3016,.T.);
#6755=EDGE_CURVE('',#5404,#5403,#4554,.T.);
#6756=EDGE_CURVE('',#5405,#5404,#3017,.T.);
#6757=EDGE_CURVE('',#5406,#5405,#4555,.T.);
#6758=EDGE_CURVE('',#5407,#5406,#3018,.T.);
#6759=EDGE_CURVE('',#5408,#5407,#3019,.T.);
#6760=EDGE_CURVE('',#5408,#5409,#3020,.T.);
#6761=EDGE_CURVE('',#5409,#5392,#4556,.T.);
#6762=EDGE_CURVE('',#5410,#5409,#3021,.T.);
#6763=EDGE_CURVE('',#5411,#5410,#204,.T.);
#6764=EDGE_CURVE('',#5394,#5411,#289,.T.);
#6765=EDGE_CURVE('',#5412,#5394,#3022,.T.);
#6766=EDGE_CURVE('',#5413,#5412,#3023,.T.);
#6767=EDGE_CURVE('',#5414,#5413,#4557,.T.);
#6768=EDGE_CURVE('',#5395,#5414,#3024,.T.);
#6769=EDGE_CURVE('',#5414,#5415,#3025,.T.);
#6770=EDGE_CURVE('',#5415,#5396,#3026,.T.);
#6771=EDGE_CURVE('',#5416,#5415,#4558,.T.);
#6772=EDGE_CURVE('',#5417,#5416,#3027,.T.);
#6773=EDGE_CURVE('',#5397,#5417,#3028,.T.);
#6774=EDGE_CURVE('',#5404,#5416,#3029,.T.);
#6775=EDGE_CURVE('',#5413,#5405,#3030,.T.);
#6776=EDGE_CURVE('',#5418,#5400,#3031,.T.);
#6777=EDGE_CURVE('',#5419,#5418,#4559,.T.);
#6778=EDGE_CURVE('',#5420,#5419,#3032,.T.);
#6779=EDGE_CURVE('',#5421,#5420,#4560,.T.);
#6780=EDGE_CURVE('',#5422,#5421,#3033,.T.);
#6781=EDGE_CURVE('',#5401,#5422,#4561,.T.);
#6782=EDGE_CURVE('',#5423,#5416,#290,.T.);
#6783=EDGE_CURVE('',#5399,#5423,#3034,.T.);
#6784=EDGE_CURVE('',#5424,#5411,#3035,.T.);
#6785=EDGE_CURVE('',#5413,#5424,#291,.T.);
#6786=EDGE_CURVE('',#5425,#5426,#4562,.T.);
#6787=EDGE_CURVE('',#5427,#5425,#3036,.T.);
#6788=EDGE_CURVE('',#5428,#5427,#4563,.T.);
#6789=EDGE_CURVE('',#5410,#5428,#3037,.T.);
#6790=EDGE_CURVE('',#5429,#5408,#4564,.T.);
#6791=EDGE_CURVE('',#5426,#5429,#3038,.T.);
#6792=EDGE_CURVE('',#5403,#5430,#3039,.T.);
#6793=EDGE_CURVE('',#5430,#5423,#4565,.T.);
#6794=EDGE_CURVE('',#5424,#5431,#4566,.T.);
#6795=EDGE_CURVE('',#5431,#5406,#3040,.T.);
#6796=EDGE_CURVE('',#5430,#5432,#3041,.T.);
#6797=EDGE_CURVE('',#5432,#5418,#3042,.T.);
#6798=EDGE_CURVE('',#5400,#5433,#3043,.T.);
#6799=EDGE_CURVE('',#5433,#5430,#3044,.T.);
#6800=EDGE_CURVE('',#5432,#5434,#4567,.T.);
#6801=EDGE_CURVE('',#5434,#5419,#3045,.T.);
#6802=EDGE_CURVE('',#5420,#5435,#3046,.T.);
#6803=EDGE_CURVE('',#5435,#5436,#4568,.T.);
#6804=EDGE_CURVE('',#5436,#5421,#3047,.T.);
#6805=EDGE_CURVE('',#5436,#5437,#3048,.T.);
#6806=EDGE_CURVE('',#5437,#5422,#3049,.T.);
#6807=EDGE_CURVE('',#5437,#5402,#4569,.T.);
#6808=EDGE_CURVE('',#5410,#5438,#3050,.T.);
#6809=EDGE_CURVE('',#5438,#5431,#3051,.T.);
#6810=EDGE_CURVE('',#5426,#5439,#3052,.T.);
#6811=EDGE_CURVE('',#5440,#5429,#3053,.T.);
#6812=EDGE_CURVE('',#5439,#5440,#3054,.T.);
#6813=EDGE_CURVE('',#5439,#5441,#4570,.T.);
#6814=EDGE_CURVE('',#5441,#5425,#3055,.T.);
#6815=EDGE_CURVE('',#5427,#5442,#3056,.T.);
#6816=EDGE_CURVE('',#5442,#5443,#4571,.T.);
#6817=EDGE_CURVE('',#5443,#5428,#3057,.T.);
#6818=EDGE_CURVE('',#5443,#5431,#3058,.T.);
#6819=EDGE_CURVE('',#5407,#5440,#4572,.T.);
#6820=EDGE_CURVE('',#5435,#5434,#3059,.T.);
#6821=EDGE_CURVE('',#5442,#5441,#3060,.T.);
#6822=EDGE_CURVE('',#5444,#5444,#4573,.T.);
#6823=EDGE_CURVE('',#5444,#5445,#3061,.T.);
#6824=EDGE_CURVE('',#5445,#5445,#4574,.T.);
#6825=EDGE_CURVE('',#5446,#5446,#4575,.T.);
#6826=EDGE_CURVE('',#5446,#5447,#3062,.T.);
#6827=EDGE_CURVE('',#5447,#5447,#4576,.T.);
#6828=EDGE_CURVE('',#5448,#5448,#4577,.T.);
#6829=EDGE_CURVE('',#5448,#5449,#3063,.T.);
#6830=EDGE_CURVE('',#5449,#5449,#4578,.T.);
#6831=EDGE_CURVE('',#5450,#5450,#4579,.T.);
#6832=EDGE_CURVE('',#5450,#5451,#3064,.T.);
#6833=EDGE_CURVE('',#5451,#5451,#4580,.T.);
#6834=EDGE_CURVE('',#5452,#5452,#4581,.T.);
#6835=EDGE_CURVE('',#5452,#5453,#3065,.T.);
#6836=EDGE_CURVE('',#5453,#5453,#4582,.T.);
#6837=EDGE_CURVE('',#5454,#5454,#4583,.T.);
#6838=EDGE_CURVE('',#5454,#5455,#3066,.T.);
#6839=EDGE_CURVE('',#5455,#5455,#4584,.T.);
#6840=EDGE_CURVE('',#5456,#5456,#4585,.T.);
#6841=EDGE_CURVE('',#5456,#5457,#3067,.T.);
#6842=EDGE_CURVE('',#5457,#5457,#4586,.T.);
#6843=EDGE_CURVE('',#5458,#5458,#4587,.T.);
#6844=EDGE_CURVE('',#5458,#5459,#3068,.T.);
#6845=EDGE_CURVE('',#5459,#5459,#4588,.T.);
#6846=EDGE_CURVE('',#5460,#5461,#4589,.T.);
#6847=EDGE_CURVE('',#5461,#5462,#3069,.T.);
#6848=EDGE_CURVE('',#5462,#5462,#4590,.T.);
#6849=EDGE_CURVE('',#5461,#5460,#4591,.T.);
#6850=EDGE_CURVE('',#5463,#5463,#4592,.T.);
#6851=EDGE_CURVE('',#5463,#5464,#3070,.T.);
#6852=EDGE_CURVE('',#5464,#5464,#4593,.T.);
#6853=EDGE_CURVE('',#5465,#5465,#4594,.T.);
#6854=EDGE_CURVE('',#5465,#5466,#3071,.T.);
#6855=EDGE_CURVE('',#5466,#5466,#4595,.T.);
#6856=EDGE_CURVE('',#5467,#5467,#4596,.T.);
#6857=EDGE_CURVE('',#5467,#5468,#3072,.T.);
#6858=EDGE_CURVE('',#5468,#5468,#4597,.T.);
#6859=EDGE_CURVE('',#5469,#5469,#4598,.T.);
#6860=EDGE_CURVE('',#5469,#5470,#3073,.T.);
#6861=EDGE_CURVE('',#5470,#5470,#4599,.T.);
#6862=EDGE_CURVE('',#5471,#5471,#4600,.T.);
#6863=EDGE_CURVE('',#5471,#5472,#3074,.T.);
#6864=EDGE_CURVE('',#5472,#5472,#4601,.T.);
#6865=EDGE_CURVE('',#5473,#5473,#4602,.T.);
#6866=EDGE_CURVE('',#5473,#5474,#3075,.T.);
#6867=EDGE_CURVE('',#5474,#5474,#4603,.T.);
#6868=EDGE_CURVE('',#5475,#5475,#4604,.T.);
#6869=EDGE_CURVE('',#5475,#5476,#3076,.T.);
#6870=EDGE_CURVE('',#5476,#5476,#4605,.T.);
#6871=EDGE_CURVE('',#5477,#5477,#4606,.T.);
#6872=EDGE_CURVE('',#5477,#5478,#3077,.T.);
#6873=EDGE_CURVE('',#5478,#5478,#4607,.T.);
#6874=EDGE_CURVE('',#5479,#5479,#4608,.T.);
#6875=EDGE_CURVE('',#5479,#5480,#3078,.T.);
#6876=EDGE_CURVE('',#5480,#5480,#4609,.T.);
#6877=EDGE_CURVE('',#5460,#5481,#3079,.T.);
#6878=EDGE_CURVE('',#5481,#5481,#4610,.T.);
#6879=EDGE_CURVE('',#5482,#5483,#3080,.T.);
#6880=EDGE_CURVE('',#5482,#5484,#4611,.T.);
#6881=EDGE_CURVE('',#5484,#5485,#3081,.T.);
#6882=EDGE_CURVE('',#5485,#5483,#4612,.T.);
#6883=EDGE_CURVE('',#5486,#5487,#4613,.T.);
#6884=EDGE_CURVE('',#5486,#5488,#3082,.T.);
#6885=EDGE_CURVE('',#5489,#5488,#4614,.T.);
#6886=EDGE_CURVE('',#5487,#5489,#3083,.T.);
#6887=EDGE_CURVE('',#5484,#5487,#3084,.T.);
#6888=EDGE_CURVE('',#5482,#5486,#3085,.T.);
#6889=EDGE_CURVE('',#5489,#5485,#3086,.T.);
#6890=EDGE_CURVE('',#5488,#5483,#3087,.T.);
#6891=EDGE_CURVE('',#5490,#5490,#4615,.T.);
#6892=EDGE_CURVE('',#5490,#5491,#3088,.T.);
#6893=EDGE_CURVE('',#5491,#5491,#4616,.T.);
#6894=EDGE_CURVE('',#5492,#5492,#4617,.T.);
#6895=EDGE_CURVE('',#5492,#5493,#3089,.T.);
#6896=EDGE_CURVE('',#5493,#5493,#4618,.T.);
#6897=EDGE_CURVE('',#5494,#5494,#4619,.T.);
#6898=EDGE_CURVE('',#5494,#5495,#3090,.T.);
#6899=EDGE_CURVE('',#5495,#5495,#4620,.T.);
#6900=EDGE_CURVE('',#5496,#5497,#4621,.T.);
#6901=EDGE_CURVE('',#5497,#5498,#3091,.T.);
#6902=EDGE_CURVE('',#5498,#5499,#4622,.T.);
#6903=EDGE_CURVE('',#5499,#5496,#3092,.T.);
#6904=EDGE_CURVE('',#5500,#5500,#4623,.T.);
#6905=EDGE_CURVE('',#5500,#5501,#3093,.T.);
#6906=EDGE_CURVE('',#5501,#5501,#4624,.T.);
#6907=EDGE_CURVE('',#5502,#5502,#4625,.T.);
#6908=EDGE_CURVE('',#5502,#5503,#3094,.T.);
#6909=EDGE_CURVE('',#5503,#5503,#4626,.T.);
#6910=EDGE_CURVE('',#5504,#5505,#3095,.T.);
#6911=EDGE_CURVE('',#5505,#5506,#3096,.T.);
#6912=EDGE_CURVE('',#5507,#5506,#3097,.T.);
#6913=EDGE_CURVE('',#5508,#5507,#3098,.T.);
#6914=EDGE_CURVE('',#5508,#5509,#3099,.T.);
#6915=EDGE_CURVE('',#5509,#5510,#3100,.T.);
#6916=EDGE_CURVE('',#5511,#5510,#3101,.T.);
#6917=EDGE_CURVE('',#5511,#5512,#3102,.T.);
#6918=EDGE_CURVE('',#5513,#5512,#3103,.T.);
#6919=EDGE_CURVE('',#5504,#5513,#3104,.T.);
#6920=EDGE_CURVE('',#5513,#5514,#3105,.T.);
#6921=EDGE_CURVE('',#5512,#5515,#3106,.T.);
#6922=EDGE_CURVE('',#5515,#5514,#3107,.T.);
#6923=EDGE_CURVE('',#5508,#5516,#3108,.T.);
#6924=EDGE_CURVE('',#5517,#5516,#3109,.T.);
#6925=EDGE_CURVE('',#5517,#5509,#3110,.T.);
#6926=EDGE_CURVE('',#5518,#5519,#3111,.T.);
#6927=EDGE_CURVE('',#5518,#5520,#3112,.T.);
#6928=EDGE_CURVE('',#5521,#5520,#3113,.T.);
#6929=EDGE_CURVE('',#5521,#5519,#3114,.T.);
#6930=EDGE_CURVE('',#5510,#5522,#3115,.T.);
#6931=EDGE_CURVE('',#5523,#5522,#3116,.T.);
#6932=EDGE_CURVE('',#5523,#5511,#3117,.T.);
#6933=EDGE_CURVE('',#5524,#5516,#3118,.T.);
#6934=EDGE_CURVE('',#5524,#5525,#3119,.T.);
#6935=EDGE_CURVE('',#5525,#5526,#3120,.T.);
#6936=EDGE_CURVE('',#5527,#5526,#3121,.T.);
#6937=EDGE_CURVE('',#5514,#5527,#3122,.T.);
#6938=EDGE_CURVE('',#5515,#5523,#3123,.T.);
#6939=EDGE_CURVE('',#5522,#5517,#3124,.T.);
#6940=EDGE_CURVE('',#5528,#5529,#3125,.T.);
#6941=EDGE_CURVE('',#5528,#5530,#3126,.T.);
#6942=EDGE_CURVE('',#5531,#5530,#3127,.T.);
#6943=EDGE_CURVE('',#5529,#5531,#3128,.T.);
#6944=EDGE_CURVE('',#5519,#5531,#4627,.T.);
#6945=EDGE_CURVE('',#5529,#5521,#4628,.T.);
#6946=EDGE_CURVE('',#5520,#5499,#4629,.T.);
#6947=EDGE_CURVE('',#5532,#5498,#3129,.T.);
#6948=EDGE_CURVE('',#5532,#5505,#4630,.T.);
#6949=EDGE_CURVE('',#5504,#5527,#3130,.T.);
#6950=EDGE_CURVE('',#5526,#5528,#4631,.T.);
#6951=EDGE_CURVE('',#5497,#5533,#3131,.T.);
#6952=EDGE_CURVE('',#5496,#5518,#4632,.T.);
#6953=EDGE_CURVE('',#5530,#5525,#4633,.T.);
#6954=EDGE_CURVE('',#5507,#5524,#3132,.T.);
#6955=EDGE_CURVE('',#5506,#5533,#4634,.T.);
#6956=EDGE_CURVE('',#5533,#5532,#3133,.T.);
#6957=EDGE_CURVE('',#5534,#5535,#3134,.T.);
#6958=EDGE_CURVE('',#5536,#5535,#3135,.T.);
#6959=EDGE_CURVE('',#5537,#5536,#3136,.T.);
#6960=EDGE_CURVE('',#5537,#5534,#3137,.T.);
#6961=EDGE_CURVE('',#5535,#5538,#3138,.T.);
#6962=EDGE_CURVE('',#5539,#5538,#3139,.T.);
#6963=EDGE_CURVE('',#5536,#5539,#3140,.T.);
#6964=EDGE_CURVE('',#5538,#5540,#3141,.T.);
#6965=EDGE_CURVE('',#5541,#5540,#3142,.T.);
#6966=EDGE_CURVE('',#5539,#5541,#3143,.T.);
#6967=EDGE_CURVE('',#5540,#5534,#3144,.T.);
#6968=EDGE_CURVE('',#5541,#5537,#3145,.T.);
#6969=EDGE_CURVE('',#5542,#5542,#4635,.T.);
#6970=EDGE_CURVE('',#5542,#5543,#3146,.T.);
#6971=EDGE_CURVE('',#5543,#5543,#4636,.T.);
#6972=EDGE_CURVE('',#5544,#5544,#4637,.T.);
#6973=EDGE_CURVE('',#5544,#5545,#3147,.T.);
#6974=EDGE_CURVE('',#5545,#5545,#4638,.T.);
#6975=EDGE_CURVE('',#5546,#5546,#4639,.T.);
#6976=EDGE_CURVE('',#5546,#5547,#3148,.T.);
#6977=EDGE_CURVE('',#5547,#5547,#4640,.T.);
#6978=EDGE_CURVE('',#5548,#5548,#4641,.T.);
#6979=EDGE_CURVE('',#5548,#5549,#3149,.T.);
#6980=EDGE_CURVE('',#5549,#5549,#4642,.T.);
#6981=EDGE_CURVE('',#5550,#5550,#4643,.T.);
#6982=EDGE_CURVE('',#5550,#5551,#3150,.T.);
#6983=EDGE_CURVE('',#5551,#5551,#4644,.T.);
#6984=EDGE_CURVE('',#5552,#5553,#3151,.T.);
#6985=EDGE_CURVE('',#5552,#5554,#3152,.T.);
#6986=EDGE_CURVE('',#5554,#5555,#3153,.T.);
#6987=EDGE_CURVE('',#5555,#5553,#3154,.T.);
#6988=EDGE_CURVE('',#5556,#5557,#3155,.T.);
#6989=EDGE_CURVE('',#5556,#5552,#3156,.T.);
#6990=EDGE_CURVE('',#5553,#5558,#3157,.T.);
#6991=EDGE_CURVE('',#5558,#5559,#3158,.T.);
#6992=EDGE_CURVE('',#5557,#5559,#3159,.T.);
#6993=EDGE_CURVE('',#5559,#5560,#3160,.T.);
#6994=EDGE_CURVE('',#5561,#5560,#3161,.T.);
#6995=EDGE_CURVE('',#5557,#5561,#3162,.T.);
#6996=EDGE_CURVE('',#5562,#5563,#3163,.T.);
#6997=EDGE_CURVE('',#5562,#5564,#3164,.T.);
#6998=EDGE_CURVE('',#5561,#5564,#3165,.T.);
#6999=EDGE_CURVE('',#5560,#5565,#3166,.T.);
#7000=EDGE_CURVE('',#5565,#5563,#3167,.T.);
#7001=EDGE_CURVE('',#5566,#5567,#3168,.T.);
#7002=EDGE_CURVE('',#5566,#5562,#3169,.T.);
#7003=EDGE_CURVE('',#5563,#5567,#3170,.T.);
#7004=EDGE_CURVE('',#5568,#5569,#3171,.T.);
#7005=EDGE_CURVE('',#5569,#5570,#3172,.T.);
#7006=EDGE_CURVE('',#5571,#5570,#3173,.T.);
#7007=EDGE_CURVE('',#5571,#5566,#3174,.T.);
#7008=EDGE_CURVE('',#5567,#5568,#3175,.T.);
#7009=EDGE_CURVE('',#5572,#5573,#3176,.T.);
#7010=EDGE_CURVE('',#5572,#5574,#3177,.T.);
#7011=EDGE_CURVE('',#5574,#5575,#3178,.T.);
#7012=EDGE_CURVE('',#5575,#5555,#3179,.T.);
#7013=EDGE_CURVE('',#5554,#5573,#3180,.T.);
#7014=EDGE_CURVE('',#5570,#5576,#3181,.T.);
#7015=EDGE_CURVE('',#5576,#5577,#3182,.T.);
#7016=EDGE_CURVE('',#5577,#5578,#3183,.T.);
#7017=EDGE_CURVE('',#5579,#5578,#3184,.T.);
#7018=EDGE_CURVE('',#5579,#5572,#3185,.T.);
#7019=EDGE_CURVE('',#5573,#5556,#3186,.T.);
#7020=EDGE_CURVE('',#5564,#5571,#3187,.T.);
#7021=EDGE_CURVE('',#5580,#5581,#3188,.T.);
#7022=EDGE_CURVE('',#5580,#5569,#3189,.T.);
#7023=EDGE_CURVE('',#5568,#5565,#3190,.T.);
#7024=EDGE_CURVE('',#5558,#5575,#3191,.T.);
#7025=EDGE_CURVE('',#5574,#5582,#3192,.T.);
#7026=EDGE_CURVE('',#5582,#5583,#3193,.T.);
#7027=EDGE_CURVE('',#5581,#5583,#3194,.T.);
#7028=EDGE_CURVE('',#5584,#5585,#4645,.T.);
#7029=EDGE_CURVE('',#5584,#5586,#3195,.T.);
#7030=EDGE_CURVE('',#5587,#5586,#4646,.T.);
#7031=EDGE_CURVE('',#5585,#5587,#3196,.T.);
#7032=EDGE_CURVE('',#5585,#5588,#3197,.T.);
#7033=EDGE_CURVE('',#5589,#5587,#3198,.T.);
#7034=EDGE_CURVE('',#5589,#5588,#3199,.T.);
#7035=EDGE_CURVE('',#5590,#5584,#3200,.T.);
#7036=EDGE_CURVE('',#5590,#5591,#3201,.T.);
#7037=EDGE_CURVE('',#5586,#5591,#3202,.T.);
#7038=EDGE_CURVE('',#5590,#5581,#4647,.T.);
#7039=EDGE_CURVE('',#5583,#5591,#4648,.T.);
#7040=EDGE_CURVE('',#5577,#5588,#4649,.T.);
#7041=EDGE_CURVE('',#5589,#5578,#4650,.T.);
#7042=EDGE_CURVE('',#5583,#5578,#3203,.T.);
#7043=EDGE_CURVE('',#5582,#5579,#3204,.T.);
#7044=EDGE_CURVE('',#5581,#5577,#3205,.T.);
#7045=EDGE_CURVE('',#5576,#5580,#3206,.T.);
#7046=EDGE_CURVE('',#5592,#5592,#4651,.T.);
#7047=EDGE_CURVE('',#5592,#5593,#4652,.T.);
#7048=EDGE_CURVE('',#5593,#5593,#4653,.T.);
#7049=EDGE_CURVE('',#5594,#5594,#4654,.T.);
#7050=EDGE_CURVE('',#5594,#5595,#3207,.T.);
#7051=EDGE_CURVE('',#5595,#5595,#4655,.T.);
#7052=EDGE_CURVE('',#5596,#5597,#4656,.T.);
#7053=EDGE_CURVE('',#5597,#5596,#4657,.T.);
#7054=EDGE_CURVE('',#5597,#5594,#3208,.T.);
#7055=EDGE_CURVE('',#5596,#5598,#3209,.T.);
#7056=EDGE_CURVE('',#5598,#5598,#4658,.T.);
#7057=EDGE_CURVE('',#5593,#5599,#3210,.T.);
#7058=EDGE_CURVE('',#5599,#5599,#4659,.T.);
#7059=EDGE_CURVE('',#5600,#5600,#4660,.T.);
#7060=EDGE_CURVE('',#5600,#5592,#3211,.T.);
#7061=EDGE_CURVE('',#5601,#5602,#4661,.T.);
#7062=EDGE_CURVE('',#5603,#5604,#4662,.T.);
#7063=EDGE_CURVE('',#5605,#5606,#4663,.T.);
#7064=EDGE_CURVE('',#5607,#5608,#4664,.T.);
#7065=EDGE_CURVE('',#5609,#5610,#4665,.T.);
#7066=EDGE_CURVE('',#5611,#5612,#4666,.T.);
#7067=EDGE_CURVE('',#5613,#5614,#4667,.T.);
#7068=EDGE_CURVE('',#5615,#5616,#4668,.T.);
#7069=EDGE_CURVE('',#5617,#5618,#4669,.T.);
#7070=EDGE_CURVE('',#5619,#5620,#4670,.T.);
#7071=EDGE_CURVE('',#5621,#5622,#4671,.T.);
#7072=EDGE_CURVE('',#5623,#5624,#4672,.T.);
#7073=EDGE_CURVE('',#5625,#5625,#4673,.T.);
#7074=EDGE_CURVE('',#5625,#5626,#3212,.T.);
#7075=EDGE_CURVE('',#5626,#5626,#4674,.T.);
#7076=EDGE_CURVE('',#5627,#5627,#4675,.T.);
#7077=EDGE_CURVE('',#5627,#5628,#3213,.T.);
#7078=EDGE_CURVE('',#5628,#5628,#4676,.T.);
#7079=EDGE_CURVE('',#5629,#5629,#4677,.T.);
#7080=EDGE_CURVE('',#5629,#5630,#3214,.T.);
#7081=EDGE_CURVE('',#5630,#5630,#4678,.T.);
#7082=EDGE_CURVE('',#5631,#5631,#4679,.T.);
#7083=EDGE_CURVE('',#5631,#5632,#3215,.T.);
#7084=EDGE_CURVE('',#5632,#5632,#4680,.T.);
#7085=EDGE_CURVE('',#5633,#5633,#4681,.T.);
#7086=EDGE_CURVE('',#5633,#5634,#3216,.T.);
#7087=EDGE_CURVE('',#5634,#5634,#4682,.T.);
#7088=EDGE_CURVE('',#5635,#5635,#4683,.T.);
#7089=EDGE_CURVE('',#5635,#5636,#3217,.T.);
#7090=EDGE_CURVE('',#5636,#5636,#4684,.T.);
#7091=EDGE_CURVE('',#5637,#5637,#4685,.T.);
#7092=EDGE_CURVE('',#5637,#5635,#4686,.T.);
#7093=EDGE_CURVE('',#5638,#5638,#4687,.T.);
#7094=EDGE_CURVE('',#5638,#5637,#3218,.T.);
#7095=EDGE_CURVE('',#5639,#5640,#4688,.T.);
#7096=EDGE_CURVE('',#5640,#5639,#4689,.T.);
#7097=EDGE_CURVE('',#5640,#5641,#3219,.T.);
#7098=EDGE_CURVE('',#5641,#5641,#4690,.T.);
#7099=EDGE_CURVE('',#5639,#5642,#3220,.T.);
#7100=EDGE_CURVE('',#5642,#5642,#4691,.T.);
#7101=EDGE_CURVE('',#5643,#5643,#4692,.T.);
#7102=EDGE_CURVE('',#5643,#5644,#3221,.T.);
#7103=EDGE_CURVE('',#5644,#5644,#4693,.T.);
#7104=EDGE_CURVE('',#5645,#5645,#4694,.T.);
#7105=EDGE_CURVE('',#5645,#5646,#3222,.T.);
#7106=EDGE_CURVE('',#5646,#5646,#4695,.T.);
#7107=EDGE_CURVE('',#5647,#5647,#4696,.T.);
#7108=EDGE_CURVE('',#5647,#5648,#3223,.T.);
#7109=EDGE_CURVE('',#5648,#5648,#4697,.T.);
#7110=EDGE_CURVE('',#5649,#5649,#4698,.T.);
#7111=EDGE_CURVE('',#5649,#5650,#3224,.T.);
#7112=EDGE_CURVE('',#5650,#5650,#4699,.T.);
#7113=EDGE_CURVE('',#5651,#5651,#4700,.T.);
#7114=EDGE_CURVE('',#5651,#5652,#3225,.T.);
#7115=EDGE_CURVE('',#5652,#5652,#4701,.T.);
#7116=EDGE_CURVE('',#5653,#5653,#4702,.T.);
#7117=EDGE_CURVE('',#5653,#5654,#3226,.T.);
#7118=EDGE_CURVE('',#5654,#5654,#4703,.T.);
#7119=EDGE_CURVE('',#5655,#5655,#4704,.T.);
#7120=EDGE_CURVE('',#5655,#5656,#3227,.T.);
#7121=EDGE_CURVE('',#5656,#5656,#4705,.T.);
#7122=EDGE_CURVE('',#5657,#5657,#4706,.T.);
#7123=EDGE_CURVE('',#5657,#5655,#3228,.T.);
#7124=EDGE_CURVE('',#5658,#5658,#4707,.T.);
#7125=EDGE_CURVE('',#5658,#5659,#3229,.T.);
#7126=EDGE_CURVE('',#5659,#5659,#4708,.T.);
#7127=EDGE_CURVE('',#5660,#5660,#4709,.T.);
#7128=EDGE_CURVE('',#5660,#5658,#3230,.T.);
#7129=EDGE_CURVE('',#5661,#5662,#4710,.T.);
#7130=EDGE_CURVE('',#5661,#5663,#3231,.T.);
#7131=EDGE_CURVE('',#5663,#5664,#4711,.T.);
#7132=EDGE_CURVE('',#5662,#5664,#3232,.T.);
#7133=EDGE_CURVE('',#5665,#5666,#4712,.T.);
#7134=EDGE_CURVE('',#5666,#5661,#3233,.T.);
#7135=EDGE_CURVE('',#5662,#5665,#3234,.T.);
#7136=EDGE_CURVE('',#5667,#5668,#4713,.T.);
#7137=EDGE_CURVE('',#5664,#5667,#3235,.T.);
#7138=EDGE_CURVE('',#5668,#5663,#3236,.T.);
#7139=EDGE_CURVE('',#5666,#5668,#3237,.T.);
#7140=EDGE_CURVE('',#5665,#5667,#3238,.T.);
#7141=EDGE_CURVE('',#5669,#5670,#3239,.T.);
#7142=EDGE_CURVE('',#5670,#5671,#4714,.T.);
#7143=EDGE_CURVE('',#5671,#5672,#4715,.T.);
#7144=EDGE_CURVE('',#5672,#5673,#4716,.T.);
#7145=EDGE_CURVE('',#5673,#5674,#4717,.T.);
#7146=EDGE_CURVE('',#5674,#5675,#4718,.T.);
#7147=EDGE_CURVE('',#5675,#5670,#4719,.T.);
#7148=EDGE_CURVE('',#5676,#5676,#4720,.T.);
#7149=EDGE_CURVE('',#5676,#5677,#4721,.T.);
#7150=EDGE_CURVE('',#5677,#5677,#4722,.T.);
#7151=EDGE_CURVE('',#5678,#5678,#4723,.T.);
#7152=EDGE_CURVE('',#5678,#5679,#3240,.T.);
#7153=EDGE_CURVE('',#5679,#5679,#4724,.T.);
#7154=EDGE_CURVE('',#5679,#5676,#3241,.T.);
#7155=EDGE_CURVE('',#5677,#5680,#3242,.T.);
#7156=EDGE_CURVE('',#5680,#5680,#4725,.T.);
#7157=EDGE_CURVE('',#5680,#5681,#3243,.T.);
#7158=EDGE_CURVE('',#5681,#5681,#4726,.T.);
#7159=EDGE_CURVE('',#5682,#5683,#3244,.T.);
#7160=EDGE_CURVE('',#5683,#5684,#3245,.T.);
#7161=EDGE_CURVE('',#5684,#5685,#3246,.T.);
#7162=EDGE_CURVE('',#5685,#5686,#3247,.T.);
#7163=EDGE_CURVE('',#5686,#5687,#3248,.T.);
#7164=EDGE_CURVE('',#5687,#5682,#3249,.T.);
#7165=EDGE_CURVE('',#5688,#5683,#3250,.T.);
#7166=EDGE_CURVE('',#5688,#5671,#3251,.T.);
#7167=EDGE_CURVE('',#5671,#5689,#3252,.T.);
#7168=EDGE_CURVE('',#5689,#5684,#3253,.T.);
#7169=EDGE_CURVE('',#5689,#5670,#3254,.T.);
#7170=EDGE_CURVE('',#5670,#5690,#3255,.T.);
#7171=EDGE_CURVE('',#5690,#5685,#3256,.T.);
#7172=EDGE_CURVE('',#5690,#5675,#3257,.T.);
#7173=EDGE_CURVE('',#5675,#5691,#3258,.T.);
#7174=EDGE_CURVE('',#5691,#5686,#3259,.T.);
#7175=EDGE_CURVE('',#5691,#5674,#3260,.T.);
#7176=EDGE_CURVE('',#5674,#5692,#3261,.T.);
#7177=EDGE_CURVE('',#5692,#5687,#3262,.T.);
#7178=EDGE_CURVE('',#5692,#5673,#3263,.T.);
#7179=EDGE_CURVE('',#5673,#5693,#3264,.T.);
#7180=EDGE_CURVE('',#5693,#5682,#3265,.T.);
#7181=EDGE_CURVE('',#5693,#5672,#3266,.T.);
#7182=EDGE_CURVE('',#5672,#5688,#3267,.T.);
#7183=ORIENTED_EDGE('',*,*,#5694,.F.);
#7184=ORIENTED_EDGE('',*,*,#5695,.T.);
#7185=ORIENTED_EDGE('',*,*,#5696,.T.);
#7186=ORIENTED_EDGE('',*,*,#5695,.F.);
#7187=ORIENTED_EDGE('',*,*,#5697,.T.);
#7188=ORIENTED_EDGE('',*,*,#5698,.T.);
#7189=ORIENTED_EDGE('',*,*,#5699,.T.);
#7190=ORIENTED_EDGE('',*,*,#5698,.F.);
#7191=ORIENTED_EDGE('',*,*,#5700,.F.);
#7192=ORIENTED_EDGE('',*,*,#5701,.T.);
#7193=ORIENTED_EDGE('',*,*,#5702,.T.);
#7194=ORIENTED_EDGE('',*,*,#5701,.F.);
#7195=ORIENTED_EDGE('',*,*,#5703,.T.);
#7196=ORIENTED_EDGE('',*,*,#5704,.T.);
#7197=ORIENTED_EDGE('',*,*,#5705,.T.);
#7198=ORIENTED_EDGE('',*,*,#5704,.F.);
#7199=ORIENTED_EDGE('',*,*,#5706,.F.);
#7200=ORIENTED_EDGE('',*,*,#5707,.T.);
#7201=ORIENTED_EDGE('',*,*,#5708,.T.);
#7202=ORIENTED_EDGE('',*,*,#5707,.F.);
#7203=ORIENTED_EDGE('',*,*,#5709,.T.);
#7204=ORIENTED_EDGE('',*,*,#5710,.T.);
#7205=ORIENTED_EDGE('',*,*,#5711,.T.);
#7206=ORIENTED_EDGE('',*,*,#5710,.F.);
#7207=ORIENTED_EDGE('',*,*,#5712,.F.);
#7208=ORIENTED_EDGE('',*,*,#5713,.T.);
#7209=ORIENTED_EDGE('',*,*,#5714,.T.);
#7210=ORIENTED_EDGE('',*,*,#5713,.F.);
#7211=ORIENTED_EDGE('',*,*,#5715,.T.);
#7212=ORIENTED_EDGE('',*,*,#5716,.T.);
#7213=ORIENTED_EDGE('',*,*,#5717,.T.);
#7214=ORIENTED_EDGE('',*,*,#5716,.F.);
#7215=ORIENTED_EDGE('',*,*,#5718,.T.);
#7216=ORIENTED_EDGE('',*,*,#5719,.T.);
#7217=ORIENTED_EDGE('',*,*,#5720,.T.);
#7218=ORIENTED_EDGE('',*,*,#5719,.F.);
#7219=ORIENTED_EDGE('',*,*,#5721,.T.);
#7220=ORIENTED_EDGE('',*,*,#5722,.T.);
#7221=ORIENTED_EDGE('',*,*,#5723,.T.);
#7222=ORIENTED_EDGE('',*,*,#5722,.F.);
#7223=ORIENTED_EDGE('',*,*,#5724,.T.);
#7224=ORIENTED_EDGE('',*,*,#5725,.T.);
#7225=ORIENTED_EDGE('',*,*,#5726,.T.);
#7226=ORIENTED_EDGE('',*,*,#5725,.F.);
#7227=ORIENTED_EDGE('',*,*,#5727,.T.);
#7228=ORIENTED_EDGE('',*,*,#5728,.T.);
#7229=ORIENTED_EDGE('',*,*,#5729,.T.);
#7230=ORIENTED_EDGE('',*,*,#5728,.F.);
#7231=ORIENTED_EDGE('',*,*,#5730,.T.);
#7232=ORIENTED_EDGE('',*,*,#5731,.T.);
#7233=ORIENTED_EDGE('',*,*,#5732,.T.);
#7234=ORIENTED_EDGE('',*,*,#5731,.F.);
#7235=ORIENTED_EDGE('',*,*,#5733,.T.);
#7236=ORIENTED_EDGE('',*,*,#5734,.T.);
#7237=ORIENTED_EDGE('',*,*,#5735,.T.);
#7238=ORIENTED_EDGE('',*,*,#5734,.F.);
#7239=ORIENTED_EDGE('',*,*,#5736,.T.);
#7240=ORIENTED_EDGE('',*,*,#5737,.T.);
#7241=ORIENTED_EDGE('',*,*,#5738,.T.);
#7242=ORIENTED_EDGE('',*,*,#5737,.F.);
#7243=ORIENTED_EDGE('',*,*,#5739,.T.);
#7244=ORIENTED_EDGE('',*,*,#5740,.T.);
#7245=ORIENTED_EDGE('',*,*,#5741,.T.);
#7246=ORIENTED_EDGE('',*,*,#5740,.F.);
#7247=ORIENTED_EDGE('',*,*,#5742,.T.);
#7248=ORIENTED_EDGE('',*,*,#5743,.T.);
#7249=ORIENTED_EDGE('',*,*,#5744,.T.);
#7250=ORIENTED_EDGE('',*,*,#5743,.F.);
#7251=ORIENTED_EDGE('',*,*,#5745,.F.);
#7252=ORIENTED_EDGE('',*,*,#5746,.F.);
#7253=ORIENTED_EDGE('',*,*,#5747,.F.);
#7254=ORIENTED_EDGE('',*,*,#5748,.T.);
#7255=ORIENTED_EDGE('',*,*,#5749,.F.);
#7256=ORIENTED_EDGE('',*,*,#5745,.T.);
#7257=ORIENTED_EDGE('',*,*,#5750,.T.);
#7258=ORIENTED_EDGE('',*,*,#5751,.T.);
#7259=ORIENTED_EDGE('',*,*,#5752,.F.);
#7260=ORIENTED_EDGE('',*,*,#5753,.T.);
#7261=ORIENTED_EDGE('',*,*,#5754,.F.);
#7262=ORIENTED_EDGE('',*,*,#5755,.F.);
#7263=ORIENTED_EDGE('',*,*,#5756,.F.);
#7264=ORIENTED_EDGE('',*,*,#5757,.T.);
#7265=ORIENTED_EDGE('',*,*,#5758,.T.);
#7266=ORIENTED_EDGE('',*,*,#5752,.T.);
#7267=ORIENTED_EDGE('',*,*,#5759,.F.);
#7268=ORIENTED_EDGE('',*,*,#5760,.F.);
#7269=ORIENTED_EDGE('',*,*,#5751,.F.);
#7270=ORIENTED_EDGE('',*,*,#5761,.T.);
#7271=ORIENTED_EDGE('',*,*,#5762,.T.);
#7272=ORIENTED_EDGE('',*,*,#5763,.T.);
#7273=ORIENTED_EDGE('',*,*,#5764,.F.);
#7274=ORIENTED_EDGE('',*,*,#5759,.T.);
#7275=ORIENTED_EDGE('',*,*,#5765,.F.);
#7276=ORIENTED_EDGE('',*,*,#5766,.T.);
#7277=ORIENTED_EDGE('',*,*,#5767,.F.);
#7278=ORIENTED_EDGE('',*,*,#5768,.F.);
#7279=ORIENTED_EDGE('',*,*,#5769,.T.);
#7280=ORIENTED_EDGE('',*,*,#5765,.T.);
#7281=ORIENTED_EDGE('',*,*,#5770,.F.);
#7282=ORIENTED_EDGE('',*,*,#5754,.T.);
#7283=ORIENTED_EDGE('',*,*,#5771,.T.);
#7284=ORIENTED_EDGE('',*,*,#5772,.T.);
#7285=ORIENTED_EDGE('',*,*,#5762,.F.);
#7286=ORIENTED_EDGE('',*,*,#5773,.T.);
#7287=ORIENTED_EDGE('',*,*,#5774,.T.);
#7288=ORIENTED_EDGE('',*,*,#5775,.T.);
#7289=ORIENTED_EDGE('',*,*,#5776,.T.);
#7290=ORIENTED_EDGE('',*,*,#5777,.T.);
#7291=ORIENTED_EDGE('',*,*,#5778,.F.);
#7292=ORIENTED_EDGE('',*,*,#5779,.T.);
#7293=ORIENTED_EDGE('',*,*,#5694,.T.);
#7294=ORIENTED_EDGE('',*,*,#5700,.T.);
#7295=ORIENTED_EDGE('',*,*,#5706,.T.);
#7296=ORIENTED_EDGE('',*,*,#5712,.T.);
#7297=ORIENTED_EDGE('',*,*,#5780,.F.);
#7298=ORIENTED_EDGE('',*,*,#5781,.T.);
#7299=ORIENTED_EDGE('',*,*,#5778,.T.);
#7300=ORIENTED_EDGE('',*,*,#5782,.T.);
#7301=ORIENTED_EDGE('',*,*,#5764,.T.);
#7302=ORIENTED_EDGE('',*,*,#5783,.T.);
#7303=ORIENTED_EDGE('',*,*,#5784,.T.);
#7304=ORIENTED_EDGE('',*,*,#5785,.T.);
#7305=ORIENTED_EDGE('',*,*,#5780,.T.);
#7306=ORIENTED_EDGE('',*,*,#5786,.T.);
#7307=ORIENTED_EDGE('',*,*,#5787,.T.);
#7308=ORIENTED_EDGE('',*,*,#5788,.T.);
#7309=ORIENTED_EDGE('',*,*,#5789,.F.);
#7310=ORIENTED_EDGE('',*,*,#5790,.F.);
#7311=ORIENTED_EDGE('',*,*,#5696,.F.);
#7312=ORIENTED_EDGE('',*,*,#5702,.F.);
#7313=ORIENTED_EDGE('',*,*,#5708,.F.);
#7314=ORIENTED_EDGE('',*,*,#5714,.F.);
#7315=ORIENTED_EDGE('',*,*,#5766,.F.);
#7316=ORIENTED_EDGE('',*,*,#5791,.F.);
#7317=ORIENTED_EDGE('',*,*,#5760,.T.);
#7318=ORIENTED_EDGE('',*,*,#5790,.T.);
#7319=ORIENTED_EDGE('',*,*,#5769,.F.);
#7320=ORIENTED_EDGE('',*,*,#5792,.F.);
#7321=ORIENTED_EDGE('',*,*,#5749,.T.);
#7322=ORIENTED_EDGE('',*,*,#5791,.T.);
#7323=ORIENTED_EDGE('',*,*,#5718,.F.);
#7324=ORIENTED_EDGE('',*,*,#5721,.F.);
#7325=ORIENTED_EDGE('',*,*,#5724,.F.);
#7326=ORIENTED_EDGE('',*,*,#5727,.F.);
#7327=ORIENTED_EDGE('',*,*,#5730,.F.);
#7328=ORIENTED_EDGE('',*,*,#5733,.F.);
#7329=ORIENTED_EDGE('',*,*,#5736,.F.);
#7330=ORIENTED_EDGE('',*,*,#5739,.F.);
#7331=ORIENTED_EDGE('',*,*,#5742,.F.);
#7332=ORIENTED_EDGE('',*,*,#5753,.F.);
#7333=ORIENTED_EDGE('',*,*,#5793,.F.);
#7334=ORIENTED_EDGE('',*,*,#5746,.T.);
#7335=ORIENTED_EDGE('',*,*,#5792,.T.);
#7336=ORIENTED_EDGE('',*,*,#5758,.F.);
#7337=ORIENTED_EDGE('',*,*,#5794,.T.);
#7338=ORIENTED_EDGE('',*,*,#5795,.T.);
#7339=ORIENTED_EDGE('',*,*,#5796,.T.);
#7340=ORIENTED_EDGE('',*,*,#5797,.F.);
#7341=ORIENTED_EDGE('',*,*,#5798,.T.);
#7342=ORIENTED_EDGE('',*,*,#5799,.T.);
#7343=ORIENTED_EDGE('',*,*,#5800,.T.);
#7344=ORIENTED_EDGE('',*,*,#5801,.T.);
#7345=ORIENTED_EDGE('',*,*,#5793,.T.);
#7346=ORIENTED_EDGE('',*,*,#5697,.F.);
#7347=ORIENTED_EDGE('',*,*,#5703,.F.);
#7348=ORIENTED_EDGE('',*,*,#5709,.F.);
#7349=ORIENTED_EDGE('',*,*,#5715,.F.);
#7350=ORIENTED_EDGE('',*,*,#5797,.T.);
#7351=ORIENTED_EDGE('',*,*,#5802,.T.);
#7352=ORIENTED_EDGE('',*,*,#5803,.F.);
#7353=ORIENTED_EDGE('',*,*,#5804,.T.);
#7354=ORIENTED_EDGE('',*,*,#5805,.T.);
#7355=ORIENTED_EDGE('',*,*,#5806,.T.);
#7356=ORIENTED_EDGE('',*,*,#5756,.T.);
#7357=ORIENTED_EDGE('',*,*,#5807,.F.);
#7358=ORIENTED_EDGE('',*,*,#5808,.F.);
#7359=ORIENTED_EDGE('',*,*,#5809,.T.);
#7360=ORIENTED_EDGE('',*,*,#5810,.T.);
#7361=ORIENTED_EDGE('',*,*,#5811,.T.);
#7362=ORIENTED_EDGE('',*,*,#5803,.T.);
#7363=ORIENTED_EDGE('',*,*,#5812,.T.);
#7364=ORIENTED_EDGE('',*,*,#5699,.F.);
#7365=ORIENTED_EDGE('',*,*,#5705,.F.);
#7366=ORIENTED_EDGE('',*,*,#5711,.F.);
#7367=ORIENTED_EDGE('',*,*,#5717,.F.);
#7368=ORIENTED_EDGE('',*,*,#5755,.T.);
#7369=ORIENTED_EDGE('',*,*,#5813,.F.);
#7370=ORIENTED_EDGE('',*,*,#5748,.F.);
#7371=ORIENTED_EDGE('',*,*,#5807,.T.);
#7372=ORIENTED_EDGE('',*,*,#5770,.T.);
#7373=ORIENTED_EDGE('',*,*,#5814,.F.);
#7374=ORIENTED_EDGE('',*,*,#5750,.F.);
#7375=ORIENTED_EDGE('',*,*,#5813,.T.);
#7376=ORIENTED_EDGE('',*,*,#5720,.F.);
#7377=ORIENTED_EDGE('',*,*,#5723,.F.);
#7378=ORIENTED_EDGE('',*,*,#5726,.F.);
#7379=ORIENTED_EDGE('',*,*,#5729,.F.);
#7380=ORIENTED_EDGE('',*,*,#5732,.F.);
#7381=ORIENTED_EDGE('',*,*,#5735,.F.);
#7382=ORIENTED_EDGE('',*,*,#5738,.F.);
#7383=ORIENTED_EDGE('',*,*,#5741,.F.);
#7384=ORIENTED_EDGE('',*,*,#5744,.F.);
#7385=ORIENTED_EDGE('',*,*,#5768,.T.);
#7386=ORIENTED_EDGE('',*,*,#5773,.F.);
#7387=ORIENTED_EDGE('',*,*,#5761,.F.);
#7388=ORIENTED_EDGE('',*,*,#5814,.T.);
#7389=ORIENTED_EDGE('',*,*,#5801,.F.);
#7390=ORIENTED_EDGE('',*,*,#5815,.T.);
#7391=ORIENTED_EDGE('',*,*,#5808,.T.);
#7392=ORIENTED_EDGE('',*,*,#5747,.T.);
#7393=ORIENTED_EDGE('',*,*,#5789,.T.);
#7394=ORIENTED_EDGE('',*,*,#5816,.T.);
#7395=ORIENTED_EDGE('',*,*,#5774,.F.);
#7396=ORIENTED_EDGE('',*,*,#5767,.T.);
#7397=ORIENTED_EDGE('',*,*,#5787,.F.);
#7398=ORIENTED_EDGE('',*,*,#5817,.T.);
#7399=ORIENTED_EDGE('',*,*,#5776,.F.);
#7400=ORIENTED_EDGE('',*,*,#5818,.T.);
#7401=ORIENTED_EDGE('',*,*,#5795,.F.);
#7402=ORIENTED_EDGE('',*,*,#5819,.T.);
#7403=ORIENTED_EDGE('',*,*,#5805,.F.);
#7404=ORIENTED_EDGE('',*,*,#5820,.T.);
#7405=ORIENTED_EDGE('',*,*,#5784,.F.);
#7406=ORIENTED_EDGE('',*,*,#5821,.T.);
#7407=ORIENTED_EDGE('',*,*,#5771,.F.);
#7408=ORIENTED_EDGE('',*,*,#5822,.T.);
#7409=ORIENTED_EDGE('',*,*,#5810,.F.);
#7410=ORIENTED_EDGE('',*,*,#5823,.T.);
#7411=ORIENTED_EDGE('',*,*,#5799,.F.);
#7412=ORIENTED_EDGE('',*,*,#5824,.T.);
#7413=ORIENTED_EDGE('',*,*,#5772,.F.);
#7414=ORIENTED_EDGE('',*,*,#5821,.F.);
#7415=ORIENTED_EDGE('',*,*,#5783,.F.);
#7416=ORIENTED_EDGE('',*,*,#5763,.F.);
#7417=ORIENTED_EDGE('',*,*,#5785,.F.);
#7418=ORIENTED_EDGE('',*,*,#5822,.F.);
#7419=ORIENTED_EDGE('',*,*,#5779,.F.);
#7420=ORIENTED_EDGE('',*,*,#5781,.F.);
#7421=ORIENTED_EDGE('',*,*,#5777,.F.);
#7422=ORIENTED_EDGE('',*,*,#5817,.F.);
#7423=ORIENTED_EDGE('',*,*,#5786,.F.);
#7424=ORIENTED_EDGE('',*,*,#5782,.F.);
#7425=ORIENTED_EDGE('',*,*,#5788,.F.);
#7426=ORIENTED_EDGE('',*,*,#5818,.F.);
#7427=ORIENTED_EDGE('',*,*,#5775,.F.);
#7428=ORIENTED_EDGE('',*,*,#5816,.F.);
#7429=ORIENTED_EDGE('',*,*,#5806,.F.);
#7430=ORIENTED_EDGE('',*,*,#5819,.F.);
#7431=ORIENTED_EDGE('',*,*,#5794,.F.);
#7432=ORIENTED_EDGE('',*,*,#5757,.F.);
#7433=ORIENTED_EDGE('',*,*,#5796,.F.);
#7434=ORIENTED_EDGE('',*,*,#5820,.F.);
#7435=ORIENTED_EDGE('',*,*,#5812,.F.);
#7436=ORIENTED_EDGE('',*,*,#5802,.F.);
#7437=ORIENTED_EDGE('',*,*,#5800,.F.);
#7438=ORIENTED_EDGE('',*,*,#5823,.F.);
#7439=ORIENTED_EDGE('',*,*,#5809,.F.);
#7440=ORIENTED_EDGE('',*,*,#5815,.F.);
#7441=ORIENTED_EDGE('',*,*,#5811,.F.);
#7442=ORIENTED_EDGE('',*,*,#5824,.F.);
#7443=ORIENTED_EDGE('',*,*,#5798,.F.);
#7444=ORIENTED_EDGE('',*,*,#5804,.F.);
#7445=ORIENTED_EDGE('',*,*,#5825,.T.);
#7446=ORIENTED_EDGE('',*,*,#5826,.T.);
#7447=ORIENTED_EDGE('',*,*,#5827,.F.);
#7448=ORIENTED_EDGE('',*,*,#5826,.F.);
#7449=ORIENTED_EDGE('',*,*,#5828,.T.);
#7450=ORIENTED_EDGE('',*,*,#5829,.T.);
#7451=ORIENTED_EDGE('',*,*,#5830,.T.);
#7452=ORIENTED_EDGE('',*,*,#5829,.F.);
#7453=ORIENTED_EDGE('',*,*,#5831,.F.);
#7454=ORIENTED_EDGE('',*,*,#5832,.T.);
#7455=ORIENTED_EDGE('',*,*,#5833,.T.);
#7456=ORIENTED_EDGE('',*,*,#5832,.F.);
#7457=ORIENTED_EDGE('',*,*,#5834,.F.);
#7458=ORIENTED_EDGE('',*,*,#5835,.T.);
#7459=ORIENTED_EDGE('',*,*,#5836,.T.);
#7460=ORIENTED_EDGE('',*,*,#5835,.F.);
#7461=ORIENTED_EDGE('',*,*,#5837,.F.);
#7462=ORIENTED_EDGE('',*,*,#5838,.T.);
#7463=ORIENTED_EDGE('',*,*,#5839,.T.);
#7464=ORIENTED_EDGE('',*,*,#5838,.F.);
#7465=ORIENTED_EDGE('',*,*,#5840,.F.);
#7466=ORIENTED_EDGE('',*,*,#5841,.T.);
#7467=ORIENTED_EDGE('',*,*,#5842,.T.);
#7468=ORIENTED_EDGE('',*,*,#5841,.F.);
#7469=ORIENTED_EDGE('',*,*,#5843,.F.);
#7470=ORIENTED_EDGE('',*,*,#5844,.T.);
#7471=ORIENTED_EDGE('',*,*,#5845,.T.);
#7472=ORIENTED_EDGE('',*,*,#5844,.F.);
#7473=ORIENTED_EDGE('',*,*,#5846,.F.);
#7474=ORIENTED_EDGE('',*,*,#5847,.T.);
#7475=ORIENTED_EDGE('',*,*,#5848,.T.);
#7476=ORIENTED_EDGE('',*,*,#5847,.F.);
#7477=ORIENTED_EDGE('',*,*,#5849,.F.);
#7478=ORIENTED_EDGE('',*,*,#5850,.T.);
#7479=ORIENTED_EDGE('',*,*,#5851,.F.);
#7480=ORIENTED_EDGE('',*,*,#5850,.F.);
#7481=ORIENTED_EDGE('',*,*,#5852,.F.);
#7482=ORIENTED_EDGE('',*,*,#5853,.T.);
#7483=ORIENTED_EDGE('',*,*,#5854,.F.);
#7484=ORIENTED_EDGE('',*,*,#5853,.F.);
#7485=ORIENTED_EDGE('',*,*,#5855,.F.);
#7486=ORIENTED_EDGE('',*,*,#5856,.T.);
#7487=ORIENTED_EDGE('',*,*,#5857,.F.);
#7488=ORIENTED_EDGE('',*,*,#5856,.F.);
#7489=ORIENTED_EDGE('',*,*,#5858,.F.);
#7490=ORIENTED_EDGE('',*,*,#5859,.T.);
#7491=ORIENTED_EDGE('',*,*,#5860,.F.);
#7492=ORIENTED_EDGE('',*,*,#5859,.F.);
#7493=ORIENTED_EDGE('',*,*,#5861,.F.);
#7494=ORIENTED_EDGE('',*,*,#5862,.T.);
#7495=ORIENTED_EDGE('',*,*,#5863,.F.);
#7496=ORIENTED_EDGE('',*,*,#5862,.F.);
#7497=ORIENTED_EDGE('',*,*,#5864,.F.);
#7498=ORIENTED_EDGE('',*,*,#5865,.T.);
#7499=ORIENTED_EDGE('',*,*,#5866,.F.);
#7500=ORIENTED_EDGE('',*,*,#5865,.F.);
#7501=ORIENTED_EDGE('',*,*,#5867,.T.);
#7502=ORIENTED_EDGE('',*,*,#5868,.T.);
#7503=ORIENTED_EDGE('',*,*,#5869,.T.);
#7504=ORIENTED_EDGE('',*,*,#5868,.F.);
#7505=ORIENTED_EDGE('',*,*,#5870,.T.);
#7506=ORIENTED_EDGE('',*,*,#5871,.T.);
#7507=ORIENTED_EDGE('',*,*,#5872,.F.);
#7508=ORIENTED_EDGE('',*,*,#5871,.F.);
#7509=ORIENTED_EDGE('',*,*,#5873,.T.);
#7510=ORIENTED_EDGE('',*,*,#5874,.T.);
#7511=ORIENTED_EDGE('',*,*,#5875,.T.);
#7512=ORIENTED_EDGE('',*,*,#5874,.F.);
#7513=ORIENTED_EDGE('',*,*,#5876,.T.);
#7514=ORIENTED_EDGE('',*,*,#5877,.T.);
#7515=ORIENTED_EDGE('',*,*,#5878,.T.);
#7516=ORIENTED_EDGE('',*,*,#5877,.F.);
#7517=ORIENTED_EDGE('',*,*,#5879,.T.);
#7518=ORIENTED_EDGE('',*,*,#5880,.T.);
#7519=ORIENTED_EDGE('',*,*,#5881,.T.);
#7520=ORIENTED_EDGE('',*,*,#5880,.F.);
#7521=ORIENTED_EDGE('',*,*,#5882,.T.);
#7522=ORIENTED_EDGE('',*,*,#5883,.T.);
#7523=ORIENTED_EDGE('',*,*,#5884,.T.);
#7524=ORIENTED_EDGE('',*,*,#5883,.F.);
#7525=ORIENTED_EDGE('',*,*,#5885,.T.);
#7526=ORIENTED_EDGE('',*,*,#5886,.T.);
#7527=ORIENTED_EDGE('',*,*,#5887,.F.);
#7528=ORIENTED_EDGE('',*,*,#5886,.F.);
#7529=ORIENTED_EDGE('',*,*,#5888,.T.);
#7530=ORIENTED_EDGE('',*,*,#5889,.T.);
#7531=ORIENTED_EDGE('',*,*,#5890,.F.);
#7532=ORIENTED_EDGE('',*,*,#5889,.F.);
#7533=ORIENTED_EDGE('',*,*,#5891,.T.);
#7534=ORIENTED_EDGE('',*,*,#5892,.T.);
#7535=ORIENTED_EDGE('',*,*,#5893,.T.);
#7536=ORIENTED_EDGE('',*,*,#5894,.T.);
#7537=ORIENTED_EDGE('',*,*,#5827,.T.);
#7538=ORIENTED_EDGE('',*,*,#5895,.T.);
#7539=ORIENTED_EDGE('',*,*,#5896,.T.);
#7540=ORIENTED_EDGE('',*,*,#5897,.T.);
#7541=ORIENTED_EDGE('',*,*,#5892,.F.);
#7542=ORIENTED_EDGE('',*,*,#5898,.T.);
#7543=ORIENTED_EDGE('',*,*,#5899,.T.);
#7544=ORIENTED_EDGE('',*,*,#5891,.F.);
#7545=ORIENTED_EDGE('',*,*,#5900,.T.);
#7546=ORIENTED_EDGE('',*,*,#5901,.T.);
#7547=ORIENTED_EDGE('',*,*,#5902,.T.);
#7548=ORIENTED_EDGE('',*,*,#5894,.F.);
#7549=ORIENTED_EDGE('',*,*,#5903,.T.);
#7550=ORIENTED_EDGE('',*,*,#5893,.F.);
#7551=ORIENTED_EDGE('',*,*,#5904,.T.);
#7552=ORIENTED_EDGE('',*,*,#5905,.T.);
#7553=ORIENTED_EDGE('',*,*,#5906,.T.);
#7554=ORIENTED_EDGE('',*,*,#5828,.F.);
#7555=ORIENTED_EDGE('',*,*,#5825,.F.);
#7556=ORIENTED_EDGE('',*,*,#5907,.F.);
#7557=ORIENTED_EDGE('',*,*,#5908,.F.);
#7558=ORIENTED_EDGE('',*,*,#5909,.T.);
#7559=ORIENTED_EDGE('',*,*,#5910,.T.);
#7560=ORIENTED_EDGE('',*,*,#5911,.T.);
#7561=ORIENTED_EDGE('',*,*,#5912,.F.);
#7562=ORIENTED_EDGE('',*,*,#5913,.T.);
#7563=ORIENTED_EDGE('',*,*,#5914,.T.);
#7564=ORIENTED_EDGE('',*,*,#5915,.T.);
#7565=ORIENTED_EDGE('',*,*,#5916,.T.);
#7566=ORIENTED_EDGE('',*,*,#5917,.T.);
#7567=ORIENTED_EDGE('',*,*,#5918,.F.);
#7568=ORIENTED_EDGE('',*,*,#5919,.T.);
#7569=ORIENTED_EDGE('',*,*,#5920,.T.);
#7570=ORIENTED_EDGE('',*,*,#5921,.T.);
#7571=ORIENTED_EDGE('',*,*,#5922,.F.);
#7572=ORIENTED_EDGE('',*,*,#5923,.F.);
#7573=ORIENTED_EDGE('',*,*,#5896,.F.);
#7574=ORIENTED_EDGE('',*,*,#5924,.T.);
#7575=ORIENTED_EDGE('',*,*,#5925,.T.);
#7576=ORIENTED_EDGE('',*,*,#5895,.F.);
#7577=ORIENTED_EDGE('',*,*,#5899,.F.);
#7578=ORIENTED_EDGE('',*,*,#5926,.T.);
#7579=ORIENTED_EDGE('',*,*,#5904,.F.);
#7580=ORIENTED_EDGE('',*,*,#5897,.F.);
#7581=ORIENTED_EDGE('',*,*,#5927,.T.);
#7582=ORIENTED_EDGE('',*,*,#5928,.T.);
#7583=ORIENTED_EDGE('',*,*,#5929,.T.);
#7584=ORIENTED_EDGE('',*,*,#5930,.T.);
#7585=ORIENTED_EDGE('',*,*,#5924,.F.);
#7586=ORIENTED_EDGE('',*,*,#5898,.F.);
#7587=ORIENTED_EDGE('',*,*,#5931,.F.);
#7588=ORIENTED_EDGE('',*,*,#5900,.F.);
#7589=ORIENTED_EDGE('',*,*,#5902,.F.);
#7590=ORIENTED_EDGE('',*,*,#5932,.T.);
#7591=ORIENTED_EDGE('',*,*,#5933,.T.);
#7592=ORIENTED_EDGE('',*,*,#5934,.T.);
#7593=ORIENTED_EDGE('',*,*,#5901,.F.);
#7594=ORIENTED_EDGE('',*,*,#5935,.F.);
#7595=ORIENTED_EDGE('',*,*,#5936,.T.);
#7596=ORIENTED_EDGE('',*,*,#5937,.T.);
#7597=ORIENTED_EDGE('',*,*,#5903,.F.);
#7598=ORIENTED_EDGE('',*,*,#5906,.F.);
#7599=ORIENTED_EDGE('',*,*,#5938,.T.);
#7600=ORIENTED_EDGE('',*,*,#5905,.F.);
#7601=ORIENTED_EDGE('',*,*,#5926,.F.);
#7602=ORIENTED_EDGE('',*,*,#5939,.T.);
#7603=ORIENTED_EDGE('',*,*,#5940,.T.);
#7604=ORIENTED_EDGE('',*,*,#5941,.T.);
#7605=ORIENTED_EDGE('',*,*,#5942,.T.);
#7606=ORIENTED_EDGE('',*,*,#5943,.T.);
#7607=ORIENTED_EDGE('',*,*,#5944,.T.);
#7608=ORIENTED_EDGE('',*,*,#5921,.F.);
#7609=ORIENTED_EDGE('',*,*,#5945,.T.);
#7610=ORIENTED_EDGE('',*,*,#5946,.T.);
#7611=ORIENTED_EDGE('',*,*,#5947,.T.);
#7612=ORIENTED_EDGE('',*,*,#5919,.F.);
#7613=ORIENTED_EDGE('',*,*,#5948,.T.);
#7614=ORIENTED_EDGE('',*,*,#5949,.T.);
#7615=ORIENTED_EDGE('',*,*,#5950,.T.);
#7616=ORIENTED_EDGE('',*,*,#5917,.F.);
#7617=ORIENTED_EDGE('',*,*,#5951,.T.);
#7618=ORIENTED_EDGE('',*,*,#5952,.F.);
#7619=ORIENTED_EDGE('',*,*,#5953,.F.);
#7620=ORIENTED_EDGE('',*,*,#5954,.F.);
#7621=ORIENTED_EDGE('',*,*,#5955,.F.);
#7622=ORIENTED_EDGE('',*,*,#5956,.F.);
#7623=ORIENTED_EDGE('',*,*,#5957,.F.);
#7624=ORIENTED_EDGE('',*,*,#5958,.F.);
#7625=ORIENTED_EDGE('',*,*,#5959,.F.);
#7626=ORIENTED_EDGE('',*,*,#5960,.F.);
#7627=ORIENTED_EDGE('',*,*,#5961,.F.);
#7628=ORIENTED_EDGE('',*,*,#5962,.F.);
#7629=ORIENTED_EDGE('',*,*,#5951,.F.);
#7630=ORIENTED_EDGE('',*,*,#5916,.F.);
#7631=ORIENTED_EDGE('',*,*,#5963,.F.);
#7632=ORIENTED_EDGE('',*,*,#5964,.F.);
#7633=ORIENTED_EDGE('',*,*,#5965,.F.);
#7634=ORIENTED_EDGE('',*,*,#5966,.F.);
#7635=ORIENTED_EDGE('',*,*,#5967,.F.);
#7636=ORIENTED_EDGE('',*,*,#5968,.F.);
#7637=ORIENTED_EDGE('',*,*,#5969,.F.);
#7638=ORIENTED_EDGE('',*,*,#5970,.F.);
#7639=ORIENTED_EDGE('',*,*,#5971,.F.);
#7640=ORIENTED_EDGE('',*,*,#5972,.F.);
#7641=ORIENTED_EDGE('',*,*,#5973,.F.);
#7642=ORIENTED_EDGE('',*,*,#5974,.F.);
#7643=ORIENTED_EDGE('',*,*,#5975,.F.);
#7644=ORIENTED_EDGE('',*,*,#5976,.F.);
#7645=ORIENTED_EDGE('',*,*,#5977,.F.);
#7646=ORIENTED_EDGE('',*,*,#5978,.F.);
#7647=ORIENTED_EDGE('',*,*,#5979,.F.);
#7648=ORIENTED_EDGE('',*,*,#5980,.F.);
#7649=ORIENTED_EDGE('',*,*,#5981,.F.);
#7650=ORIENTED_EDGE('',*,*,#5982,.F.);
#7651=ORIENTED_EDGE('',*,*,#5983,.F.);
#7652=ORIENTED_EDGE('',*,*,#5984,.F.);
#7653=ORIENTED_EDGE('',*,*,#5985,.F.);
#7654=ORIENTED_EDGE('',*,*,#5914,.F.);
#7655=ORIENTED_EDGE('',*,*,#5986,.F.);
#7656=ORIENTED_EDGE('',*,*,#5987,.F.);
#7657=ORIENTED_EDGE('',*,*,#5988,.F.);
#7658=ORIENTED_EDGE('',*,*,#5833,.F.);
#7659=ORIENTED_EDGE('',*,*,#5836,.F.);
#7660=ORIENTED_EDGE('',*,*,#5839,.F.);
#7661=ORIENTED_EDGE('',*,*,#5842,.F.);
#7662=ORIENTED_EDGE('',*,*,#5845,.F.);
#7663=ORIENTED_EDGE('',*,*,#5848,.F.);
#7664=ORIENTED_EDGE('',*,*,#5989,.T.);
#7665=ORIENTED_EDGE('',*,*,#5915,.F.);
#7666=ORIENTED_EDGE('',*,*,#5990,.T.);
#7667=ORIENTED_EDGE('',*,*,#5991,.T.);
#7668=ORIENTED_EDGE('',*,*,#5913,.F.);
#7669=ORIENTED_EDGE('',*,*,#5992,.T.);
#7670=ORIENTED_EDGE('',*,*,#5993,.T.);
#7671=ORIENTED_EDGE('',*,*,#5986,.T.);
#7672=ORIENTED_EDGE('',*,*,#5911,.F.);
#7673=ORIENTED_EDGE('',*,*,#5994,.T.);
#7674=ORIENTED_EDGE('',*,*,#5995,.T.);
#7675=ORIENTED_EDGE('',*,*,#5996,.T.);
#7676=ORIENTED_EDGE('',*,*,#5909,.F.);
#7677=ORIENTED_EDGE('',*,*,#5997,.T.);
#7678=ORIENTED_EDGE('',*,*,#5998,.T.);
#7679=ORIENTED_EDGE('',*,*,#5999,.T.);
#7680=ORIENTED_EDGE('',*,*,#5907,.T.);
#7681=ORIENTED_EDGE('',*,*,#5925,.F.);
#7682=ORIENTED_EDGE('',*,*,#5930,.F.);
#7683=ORIENTED_EDGE('',*,*,#6000,.T.);
#7684=ORIENTED_EDGE('',*,*,#5939,.F.);
#7685=ORIENTED_EDGE('',*,*,#5927,.F.);
#7686=ORIENTED_EDGE('',*,*,#5923,.T.);
#7687=ORIENTED_EDGE('',*,*,#6001,.T.);
#7688=ORIENTED_EDGE('',*,*,#6002,.T.);
#7689=ORIENTED_EDGE('',*,*,#6003,.T.);
#7690=ORIENTED_EDGE('',*,*,#6004,.T.);
#7691=ORIENTED_EDGE('',*,*,#6005,.T.);
#7692=ORIENTED_EDGE('',*,*,#5997,.F.);
#7693=ORIENTED_EDGE('',*,*,#5908,.T.);
#7694=ORIENTED_EDGE('',*,*,#6000,.F.);
#7695=ORIENTED_EDGE('',*,*,#5929,.F.);
#7696=ORIENTED_EDGE('',*,*,#6006,.T.);
#7697=ORIENTED_EDGE('',*,*,#5937,.F.);
#7698=ORIENTED_EDGE('',*,*,#6007,.T.);
#7699=ORIENTED_EDGE('',*,*,#5940,.F.);
#7700=ORIENTED_EDGE('',*,*,#6001,.F.);
#7701=ORIENTED_EDGE('',*,*,#5922,.T.);
#7702=ORIENTED_EDGE('',*,*,#5944,.F.);
#7703=ORIENTED_EDGE('',*,*,#6008,.T.);
#7704=ORIENTED_EDGE('',*,*,#6009,.T.);
#7705=ORIENTED_EDGE('',*,*,#6010,.T.);
#7706=ORIENTED_EDGE('',*,*,#6011,.T.);
#7707=ORIENTED_EDGE('',*,*,#6012,.T.);
#7708=ORIENTED_EDGE('',*,*,#6013,.T.);
#7709=ORIENTED_EDGE('',*,*,#6014,.T.);
#7710=ORIENTED_EDGE('',*,*,#6015,.T.);
#7711=ORIENTED_EDGE('',*,*,#6016,.T.);
#7712=ORIENTED_EDGE('',*,*,#5849,.T.);
#7713=ORIENTED_EDGE('',*,*,#5852,.T.);
#7714=ORIENTED_EDGE('',*,*,#5855,.T.);
#7715=ORIENTED_EDGE('',*,*,#5858,.T.);
#7716=ORIENTED_EDGE('',*,*,#5861,.T.);
#7717=ORIENTED_EDGE('',*,*,#5864,.T.);
#7718=ORIENTED_EDGE('',*,*,#6006,.F.);
#7719=ORIENTED_EDGE('',*,*,#5928,.F.);
#7720=ORIENTED_EDGE('',*,*,#6017,.T.);
#7721=ORIENTED_EDGE('',*,*,#5933,.F.);
#7722=ORIENTED_EDGE('',*,*,#5934,.F.);
#7723=ORIENTED_EDGE('',*,*,#6017,.F.);
#7724=ORIENTED_EDGE('',*,*,#5931,.T.);
#7725=ORIENTED_EDGE('',*,*,#5932,.F.);
#7726=ORIENTED_EDGE('',*,*,#6007,.F.);
#7727=ORIENTED_EDGE('',*,*,#5936,.F.);
#7728=ORIENTED_EDGE('',*,*,#6018,.T.);
#7729=ORIENTED_EDGE('',*,*,#5941,.F.);
#7730=ORIENTED_EDGE('',*,*,#5942,.F.);
#7731=ORIENTED_EDGE('',*,*,#6018,.F.);
#7732=ORIENTED_EDGE('',*,*,#5935,.T.);
#7733=ORIENTED_EDGE('',*,*,#5938,.F.);
#7734=ORIENTED_EDGE('',*,*,#5830,.F.);
#7735=ORIENTED_EDGE('',*,*,#5867,.F.);
#7736=ORIENTED_EDGE('',*,*,#6019,.T.);
#7737=ORIENTED_EDGE('',*,*,#6020,.F.);
#7738=ORIENTED_EDGE('',*,*,#6021,.T.);
#7739=ORIENTED_EDGE('',*,*,#6008,.F.);
#7740=ORIENTED_EDGE('',*,*,#5943,.F.);
#7741=ORIENTED_EDGE('',*,*,#6022,.T.);
#7742=ORIENTED_EDGE('',*,*,#6023,.T.);
#7743=ORIENTED_EDGE('',*,*,#6024,.T.);
#7744=ORIENTED_EDGE('',*,*,#5920,.F.);
#7745=ORIENTED_EDGE('',*,*,#5947,.F.);
#7746=ORIENTED_EDGE('',*,*,#6025,.F.);
#7747=ORIENTED_EDGE('',*,*,#6026,.F.);
#7748=ORIENTED_EDGE('',*,*,#6022,.F.);
#7749=ORIENTED_EDGE('',*,*,#5945,.F.);
#7750=ORIENTED_EDGE('',*,*,#6027,.T.);
#7751=ORIENTED_EDGE('',*,*,#6028,.T.);
#7752=ORIENTED_EDGE('',*,*,#6029,.T.);
#7753=ORIENTED_EDGE('',*,*,#6030,.T.);
#7754=ORIENTED_EDGE('',*,*,#6031,.T.);
#7755=ORIENTED_EDGE('',*,*,#6032,.T.);
#7756=ORIENTED_EDGE('',*,*,#6033,.T.);
#7757=ORIENTED_EDGE('',*,*,#6034,.T.);
#7758=ORIENTED_EDGE('',*,*,#6035,.T.);
#7759=ORIENTED_EDGE('',*,*,#6036,.T.);
#7760=ORIENTED_EDGE('',*,*,#6037,.T.);
#7761=ORIENTED_EDGE('',*,*,#6038,.T.);
#7762=ORIENTED_EDGE('',*,*,#6039,.T.);
#7763=ORIENTED_EDGE('',*,*,#6040,.T.);
#7764=ORIENTED_EDGE('',*,*,#6041,.T.);
#7765=ORIENTED_EDGE('',*,*,#6025,.T.);
#7766=ORIENTED_EDGE('',*,*,#5946,.F.);
#7767=ORIENTED_EDGE('',*,*,#6042,.T.);
#7768=ORIENTED_EDGE('',*,*,#6043,.T.);
#7769=ORIENTED_EDGE('',*,*,#6044,.T.);
#7770=ORIENTED_EDGE('',*,*,#6045,.T.);
#7771=ORIENTED_EDGE('',*,*,#6046,.T.);
#7772=ORIENTED_EDGE('',*,*,#6047,.T.);
#7773=ORIENTED_EDGE('',*,*,#6048,.T.);
#7774=ORIENTED_EDGE('',*,*,#6049,.T.);
#7775=ORIENTED_EDGE('',*,*,#6050,.T.);
#7776=ORIENTED_EDGE('',*,*,#6051,.T.);
#7777=ORIENTED_EDGE('',*,*,#6052,.T.);
#7778=ORIENTED_EDGE('',*,*,#6053,.T.);
#7779=ORIENTED_EDGE('',*,*,#6054,.T.);
#7780=ORIENTED_EDGE('',*,*,#6055,.T.);
#7781=ORIENTED_EDGE('',*,*,#6056,.T.);
#7782=ORIENTED_EDGE('',*,*,#6057,.T.);
#7783=ORIENTED_EDGE('',*,*,#6058,.T.);
#7784=ORIENTED_EDGE('',*,*,#6059,.T.);
#7785=ORIENTED_EDGE('',*,*,#6060,.T.);
#7786=ORIENTED_EDGE('',*,*,#6061,.T.);
#7787=ORIENTED_EDGE('',*,*,#6062,.T.);
#7788=ORIENTED_EDGE('',*,*,#6063,.T.);
#7789=ORIENTED_EDGE('',*,*,#6064,.T.);
#7790=ORIENTED_EDGE('',*,*,#5948,.F.);
#7791=ORIENTED_EDGE('',*,*,#5918,.T.);
#7792=ORIENTED_EDGE('',*,*,#5950,.F.);
#7793=ORIENTED_EDGE('',*,*,#6065,.T.);
#7794=ORIENTED_EDGE('',*,*,#6066,.T.);
#7795=ORIENTED_EDGE('',*,*,#6042,.F.);
#7796=ORIENTED_EDGE('',*,*,#6067,.T.);
#7797=ORIENTED_EDGE('',*,*,#6068,.F.);
#7798=ORIENTED_EDGE('',*,*,#6069,.F.);
#7799=ORIENTED_EDGE('',*,*,#6070,.F.);
#7800=ORIENTED_EDGE('',*,*,#6065,.F.);
#7801=ORIENTED_EDGE('',*,*,#5949,.F.);
#7802=ORIENTED_EDGE('',*,*,#5962,.T.);
#7803=ORIENTED_EDGE('',*,*,#6071,.F.);
#7804=ORIENTED_EDGE('',*,*,#6072,.T.);
#7805=ORIENTED_EDGE('',*,*,#6073,.T.);
#7806=ORIENTED_EDGE('',*,*,#6074,.T.);
#7807=ORIENTED_EDGE('',*,*,#5988,.T.);
#7808=ORIENTED_EDGE('',*,*,#6075,.F.);
#7809=ORIENTED_EDGE('',*,*,#6076,.F.);
#7810=ORIENTED_EDGE('',*,*,#6077,.F.);
#7811=ORIENTED_EDGE('',*,*,#6078,.F.);
#7812=ORIENTED_EDGE('',*,*,#6079,.F.);
#7813=ORIENTED_EDGE('',*,*,#6080,.F.);
#7814=ORIENTED_EDGE('',*,*,#6081,.F.);
#7815=ORIENTED_EDGE('',*,*,#6082,.F.);
#7816=ORIENTED_EDGE('',*,*,#6083,.F.);
#7817=ORIENTED_EDGE('',*,*,#6084,.F.);
#7818=ORIENTED_EDGE('',*,*,#6085,.F.);
#7819=ORIENTED_EDGE('',*,*,#6086,.F.);
#7820=ORIENTED_EDGE('',*,*,#6087,.F.);
#7821=ORIENTED_EDGE('',*,*,#6088,.F.);
#7822=ORIENTED_EDGE('',*,*,#5952,.T.);
#7823=ORIENTED_EDGE('',*,*,#6074,.F.);
#7824=ORIENTED_EDGE('',*,*,#6088,.T.);
#7825=ORIENTED_EDGE('',*,*,#6089,.T.);
#7826=ORIENTED_EDGE('',*,*,#6090,.T.);
#7827=ORIENTED_EDGE('',*,*,#5953,.T.);
#7828=ORIENTED_EDGE('',*,*,#6091,.F.);
#7829=ORIENTED_EDGE('',*,*,#6092,.F.);
#7830=ORIENTED_EDGE('',*,*,#5954,.T.);
#7831=ORIENTED_EDGE('',*,*,#6090,.F.);
#7832=ORIENTED_EDGE('',*,*,#6093,.T.);
#7833=ORIENTED_EDGE('',*,*,#6094,.T.);
#7834=ORIENTED_EDGE('',*,*,#6095,.T.);
#7835=ORIENTED_EDGE('',*,*,#5955,.T.);
#7836=ORIENTED_EDGE('',*,*,#6092,.T.);
#7837=ORIENTED_EDGE('',*,*,#6096,.T.);
#7838=ORIENTED_EDGE('',*,*,#6097,.F.);
#7839=ORIENTED_EDGE('',*,*,#6098,.F.);
#7840=ORIENTED_EDGE('',*,*,#6099,.F.);
#7841=ORIENTED_EDGE('',*,*,#6100,.F.);
#7842=ORIENTED_EDGE('',*,*,#6101,.F.);
#7843=ORIENTED_EDGE('',*,*,#6102,.F.);
#7844=ORIENTED_EDGE('',*,*,#6103,.F.);
#7845=ORIENTED_EDGE('',*,*,#6104,.F.);
#7846=ORIENTED_EDGE('',*,*,#6105,.F.);
#7847=ORIENTED_EDGE('',*,*,#6106,.F.);
#7848=ORIENTED_EDGE('',*,*,#5956,.T.);
#7849=ORIENTED_EDGE('',*,*,#6095,.F.);
#7850=ORIENTED_EDGE('',*,*,#6107,.T.);
#7851=ORIENTED_EDGE('',*,*,#6108,.T.);
#7852=ORIENTED_EDGE('',*,*,#6109,.T.);
#7853=ORIENTED_EDGE('',*,*,#5957,.T.);
#7854=ORIENTED_EDGE('',*,*,#6106,.T.);
#7855=ORIENTED_EDGE('',*,*,#6110,.T.);
#7856=ORIENTED_EDGE('',*,*,#6111,.F.);
#7857=ORIENTED_EDGE('',*,*,#6112,.F.);
#7858=ORIENTED_EDGE('',*,*,#5958,.T.);
#7859=ORIENTED_EDGE('',*,*,#6109,.F.);
#7860=ORIENTED_EDGE('',*,*,#6112,.T.);
#7861=ORIENTED_EDGE('',*,*,#6113,.T.);
#7862=ORIENTED_EDGE('',*,*,#6114,.T.);
#7863=ORIENTED_EDGE('',*,*,#5959,.T.);
#7864=ORIENTED_EDGE('',*,*,#6115,.F.);
#7865=ORIENTED_EDGE('',*,*,#6116,.F.);
#7866=ORIENTED_EDGE('',*,*,#6117,.F.);
#7867=ORIENTED_EDGE('',*,*,#6118,.F.);
#7868=ORIENTED_EDGE('',*,*,#6119,.F.);
#7869=ORIENTED_EDGE('',*,*,#6120,.F.);
#7870=ORIENTED_EDGE('',*,*,#6121,.F.);
#7871=ORIENTED_EDGE('',*,*,#6122,.F.);
#7872=ORIENTED_EDGE('',*,*,#6123,.F.);
#7873=ORIENTED_EDGE('',*,*,#6124,.F.);
#7874=ORIENTED_EDGE('',*,*,#6125,.F.);
#7875=ORIENTED_EDGE('',*,*,#6126,.F.);
#7876=ORIENTED_EDGE('',*,*,#6127,.F.);
#7877=ORIENTED_EDGE('',*,*,#6128,.F.);
#7878=ORIENTED_EDGE('',*,*,#5960,.T.);
#7879=ORIENTED_EDGE('',*,*,#6114,.F.);
#7880=ORIENTED_EDGE('',*,*,#6128,.T.);
#7881=ORIENTED_EDGE('',*,*,#6129,.T.);
#7882=ORIENTED_EDGE('',*,*,#6071,.T.);
#7883=ORIENTED_EDGE('',*,*,#5961,.T.);
#7884=ORIENTED_EDGE('',*,*,#5989,.F.);
#7885=ORIENTED_EDGE('',*,*,#6130,.T.);
#7886=ORIENTED_EDGE('',*,*,#6131,.T.);
#7887=ORIENTED_EDGE('',*,*,#5963,.T.);
#7888=ORIENTED_EDGE('',*,*,#6132,.F.);
#7889=ORIENTED_EDGE('',*,*,#6133,.F.);
#7890=ORIENTED_EDGE('',*,*,#5964,.T.);
#7891=ORIENTED_EDGE('',*,*,#6131,.F.);
#7892=ORIENTED_EDGE('',*,*,#6134,.F.);
#7893=ORIENTED_EDGE('',*,*,#5965,.T.);
#7894=ORIENTED_EDGE('',*,*,#6133,.T.);
#7895=ORIENTED_EDGE('',*,*,#6135,.F.);
#7896=ORIENTED_EDGE('',*,*,#6136,.F.);
#7897=ORIENTED_EDGE('',*,*,#6137,.F.);
#7898=ORIENTED_EDGE('',*,*,#5966,.T.);
#7899=ORIENTED_EDGE('',*,*,#6134,.T.);
#7900=ORIENTED_EDGE('',*,*,#6138,.F.);
#7901=ORIENTED_EDGE('',*,*,#5967,.T.);
#7902=ORIENTED_EDGE('',*,*,#6137,.T.);
#7903=ORIENTED_EDGE('',*,*,#6139,.F.);
#7904=ORIENTED_EDGE('',*,*,#6140,.T.);
#7905=ORIENTED_EDGE('',*,*,#6140,.F.);
#7906=ORIENTED_EDGE('',*,*,#6141,.F.);
#7907=ORIENTED_EDGE('',*,*,#6142,.T.);
#7908=ORIENTED_EDGE('',*,*,#6143,.F.);
#7909=ORIENTED_EDGE('',*,*,#6144,.T.);
#7910=ORIENTED_EDGE('',*,*,#5968,.T.);
#7911=ORIENTED_EDGE('',*,*,#5969,.T.);
#7912=ORIENTED_EDGE('',*,*,#6144,.F.);
#7913=ORIENTED_EDGE('',*,*,#6145,.F.);
#7914=ORIENTED_EDGE('',*,*,#6146,.T.);
#7915=ORIENTED_EDGE('',*,*,#6147,.F.);
#7916=ORIENTED_EDGE('',*,*,#5970,.T.);
#7917=ORIENTED_EDGE('',*,*,#6146,.F.);
#7918=ORIENTED_EDGE('',*,*,#6148,.F.);
#7919=ORIENTED_EDGE('',*,*,#6149,.F.);
#7920=ORIENTED_EDGE('',*,*,#6150,.F.);
#7921=ORIENTED_EDGE('',*,*,#5971,.T.);
#7922=ORIENTED_EDGE('',*,*,#6147,.T.);
#7923=ORIENTED_EDGE('',*,*,#6151,.F.);
#7924=ORIENTED_EDGE('',*,*,#6152,.F.);
#7925=ORIENTED_EDGE('',*,*,#6153,.F.);
#7926=ORIENTED_EDGE('',*,*,#5972,.T.);
#7927=ORIENTED_EDGE('',*,*,#6150,.T.);
#7928=ORIENTED_EDGE('',*,*,#6154,.F.);
#7929=ORIENTED_EDGE('',*,*,#5973,.T.);
#7930=ORIENTED_EDGE('',*,*,#6153,.T.);
#7931=ORIENTED_EDGE('',*,*,#6155,.F.);
#7932=ORIENTED_EDGE('',*,*,#6156,.T.);
#7933=ORIENTED_EDGE('',*,*,#6156,.F.);
#7934=ORIENTED_EDGE('',*,*,#6157,.F.);
#7935=ORIENTED_EDGE('',*,*,#6158,.T.);
#7936=ORIENTED_EDGE('',*,*,#6159,.F.);
#7937=ORIENTED_EDGE('',*,*,#6160,.T.);
#7938=ORIENTED_EDGE('',*,*,#5974,.T.);
#7939=ORIENTED_EDGE('',*,*,#5975,.T.);
#7940=ORIENTED_EDGE('',*,*,#6160,.F.);
#7941=ORIENTED_EDGE('',*,*,#6161,.F.);
#7942=ORIENTED_EDGE('',*,*,#6162,.T.);
#7943=ORIENTED_EDGE('',*,*,#6163,.F.);
#7944=ORIENTED_EDGE('',*,*,#5976,.T.);
#7945=ORIENTED_EDGE('',*,*,#6162,.F.);
#7946=ORIENTED_EDGE('',*,*,#6164,.F.);
#7947=ORIENTED_EDGE('',*,*,#6165,.F.);
#7948=ORIENTED_EDGE('',*,*,#6166,.F.);
#7949=ORIENTED_EDGE('',*,*,#5977,.T.);
#7950=ORIENTED_EDGE('',*,*,#6163,.T.);
#7951=ORIENTED_EDGE('',*,*,#6167,.F.);
#7952=ORIENTED_EDGE('',*,*,#6168,.F.);
#7953=ORIENTED_EDGE('',*,*,#6169,.F.);
#7954=ORIENTED_EDGE('',*,*,#5978,.T.);
#7955=ORIENTED_EDGE('',*,*,#6166,.T.);
#7956=ORIENTED_EDGE('',*,*,#6170,.F.);
#7957=ORIENTED_EDGE('',*,*,#5979,.T.);
#7958=ORIENTED_EDGE('',*,*,#6169,.T.);
#7959=ORIENTED_EDGE('',*,*,#6171,.F.);
#7960=ORIENTED_EDGE('',*,*,#6172,.T.);
#7961=ORIENTED_EDGE('',*,*,#6172,.F.);
#7962=ORIENTED_EDGE('',*,*,#6173,.F.);
#7963=ORIENTED_EDGE('',*,*,#6174,.T.);
#7964=ORIENTED_EDGE('',*,*,#6175,.F.);
#7965=ORIENTED_EDGE('',*,*,#6176,.T.);
#7966=ORIENTED_EDGE('',*,*,#5980,.T.);
#7967=ORIENTED_EDGE('',*,*,#5981,.T.);
#7968=ORIENTED_EDGE('',*,*,#6176,.F.);
#7969=ORIENTED_EDGE('',*,*,#6177,.F.);
#7970=ORIENTED_EDGE('',*,*,#6178,.T.);
#7971=ORIENTED_EDGE('',*,*,#6179,.F.);
#7972=ORIENTED_EDGE('',*,*,#5982,.T.);
#7973=ORIENTED_EDGE('',*,*,#6178,.F.);
#7974=ORIENTED_EDGE('',*,*,#6180,.F.);
#7975=ORIENTED_EDGE('',*,*,#6181,.F.);
#7976=ORIENTED_EDGE('',*,*,#6182,.F.);
#7977=ORIENTED_EDGE('',*,*,#5983,.T.);
#7978=ORIENTED_EDGE('',*,*,#6179,.T.);
#7979=ORIENTED_EDGE('',*,*,#6183,.F.);
#7980=ORIENTED_EDGE('',*,*,#5984,.T.);
#7981=ORIENTED_EDGE('',*,*,#6182,.T.);
#7982=ORIENTED_EDGE('',*,*,#6184,.F.);
#7983=ORIENTED_EDGE('',*,*,#6185,.F.);
#7984=ORIENTED_EDGE('',*,*,#6185,.T.);
#7985=ORIENTED_EDGE('',*,*,#6186,.T.);
#7986=ORIENTED_EDGE('',*,*,#5990,.F.);
#7987=ORIENTED_EDGE('',*,*,#5985,.T.);
#7988=ORIENTED_EDGE('',*,*,#5987,.T.);
#7989=ORIENTED_EDGE('',*,*,#5993,.F.);
#7990=ORIENTED_EDGE('',*,*,#6187,.F.);
#7991=ORIENTED_EDGE('',*,*,#6188,.F.);
#7992=ORIENTED_EDGE('',*,*,#6189,.F.);
#7993=ORIENTED_EDGE('',*,*,#6190,.F.);
#7994=ORIENTED_EDGE('',*,*,#6191,.F.);
#7995=ORIENTED_EDGE('',*,*,#6072,.F.);
#7996=ORIENTED_EDGE('',*,*,#6192,.F.);
#7997=ORIENTED_EDGE('',*,*,#6193,.F.);
#7998=ORIENTED_EDGE('',*,*,#6194,.F.);
#7999=ORIENTED_EDGE('',*,*,#6195,.F.);
#8000=ORIENTED_EDGE('',*,*,#6196,.F.);
#8001=ORIENTED_EDGE('',*,*,#6197,.F.);
#8002=ORIENTED_EDGE('',*,*,#6198,.F.);
#8003=ORIENTED_EDGE('',*,*,#6199,.F.);
#8004=ORIENTED_EDGE('',*,*,#6200,.F.);
#8005=ORIENTED_EDGE('',*,*,#6201,.F.);
#8006=ORIENTED_EDGE('',*,*,#6202,.F.);
#8007=ORIENTED_EDGE('',*,*,#6203,.F.);
#8008=ORIENTED_EDGE('',*,*,#6204,.F.);
#8009=ORIENTED_EDGE('',*,*,#6205,.F.);
#8010=ORIENTED_EDGE('',*,*,#5991,.F.);
#8011=ORIENTED_EDGE('',*,*,#6206,.F.);
#8012=ORIENTED_EDGE('',*,*,#5870,.F.);
#8013=ORIENTED_EDGE('',*,*,#6207,.T.);
#8014=ORIENTED_EDGE('',*,*,#6187,.T.);
#8015=ORIENTED_EDGE('',*,*,#5992,.F.);
#8016=ORIENTED_EDGE('',*,*,#5912,.T.);
#8017=ORIENTED_EDGE('',*,*,#5996,.F.);
#8018=ORIENTED_EDGE('',*,*,#6208,.T.);
#8019=ORIENTED_EDGE('',*,*,#6209,.F.);
#8020=ORIENTED_EDGE('',*,*,#6210,.F.);
#8021=ORIENTED_EDGE('',*,*,#6211,.F.);
#8022=ORIENTED_EDGE('',*,*,#5994,.F.);
#8023=ORIENTED_EDGE('',*,*,#5910,.F.);
#8024=ORIENTED_EDGE('',*,*,#5999,.F.);
#8025=ORIENTED_EDGE('',*,*,#6212,.T.);
#8026=ORIENTED_EDGE('',*,*,#6213,.T.);
#8027=ORIENTED_EDGE('',*,*,#6214,.T.);
#8028=ORIENTED_EDGE('',*,*,#6215,.T.);
#8029=ORIENTED_EDGE('',*,*,#6216,.T.);
#8030=ORIENTED_EDGE('',*,*,#6217,.T.);
#8031=ORIENTED_EDGE('',*,*,#6218,.T.);
#8032=ORIENTED_EDGE('',*,*,#6219,.T.);
#8033=ORIENTED_EDGE('',*,*,#6220,.T.);
#8034=ORIENTED_EDGE('',*,*,#6221,.T.);
#8035=ORIENTED_EDGE('',*,*,#6222,.T.);
#8036=ORIENTED_EDGE('',*,*,#6223,.T.);
#8037=ORIENTED_EDGE('',*,*,#6224,.T.);
#8038=ORIENTED_EDGE('',*,*,#6225,.T.);
#8039=ORIENTED_EDGE('',*,*,#6226,.T.);
#8040=ORIENTED_EDGE('',*,*,#6227,.T.);
#8041=ORIENTED_EDGE('',*,*,#6228,.T.);
#8042=ORIENTED_EDGE('',*,*,#6229,.T.);
#8043=ORIENTED_EDGE('',*,*,#6230,.T.);
#8044=ORIENTED_EDGE('',*,*,#6231,.T.);
#8045=ORIENTED_EDGE('',*,*,#6232,.T.);
#8046=ORIENTED_EDGE('',*,*,#6233,.T.);
#8047=ORIENTED_EDGE('',*,*,#6234,.T.);
#8048=ORIENTED_EDGE('',*,*,#6235,.T.);
#8049=ORIENTED_EDGE('',*,*,#6236,.T.);
#8050=ORIENTED_EDGE('',*,*,#6237,.T.);
#8051=ORIENTED_EDGE('',*,*,#6238,.T.);
#8052=ORIENTED_EDGE('',*,*,#6208,.F.);
#8053=ORIENTED_EDGE('',*,*,#5995,.F.);
#8054=ORIENTED_EDGE('',*,*,#6211,.T.);
#8055=ORIENTED_EDGE('',*,*,#6239,.T.);
#8056=ORIENTED_EDGE('',*,*,#6240,.T.);
#8057=ORIENTED_EDGE('',*,*,#6241,.T.);
#8058=ORIENTED_EDGE('',*,*,#6242,.T.);
#8059=ORIENTED_EDGE('',*,*,#6243,.T.);
#8060=ORIENTED_EDGE('',*,*,#6244,.T.);
#8061=ORIENTED_EDGE('',*,*,#6245,.T.);
#8062=ORIENTED_EDGE('',*,*,#6246,.T.);
#8063=ORIENTED_EDGE('',*,*,#6247,.T.);
#8064=ORIENTED_EDGE('',*,*,#6248,.T.);
#8065=ORIENTED_EDGE('',*,*,#5998,.F.);
#8066=ORIENTED_EDGE('',*,*,#6005,.F.);
#8067=ORIENTED_EDGE('',*,*,#6249,.T.);
#8068=ORIENTED_EDGE('',*,*,#6250,.F.);
#8069=ORIENTED_EDGE('',*,*,#6251,.T.);
#8070=ORIENTED_EDGE('',*,*,#6252,.T.);
#8071=ORIENTED_EDGE('',*,*,#6253,.T.);
#8072=ORIENTED_EDGE('',*,*,#6209,.T.);
#8073=ORIENTED_EDGE('',*,*,#6254,.T.);
#8074=ORIENTED_EDGE('',*,*,#6255,.T.);
#8075=ORIENTED_EDGE('',*,*,#6256,.T.);
#8076=ORIENTED_EDGE('',*,*,#6003,.F.);
#8077=ORIENTED_EDGE('',*,*,#6257,.T.);
#8078=ORIENTED_EDGE('',*,*,#6258,.T.);
#8079=ORIENTED_EDGE('',*,*,#6259,.T.);
#8080=ORIENTED_EDGE('',*,*,#6260,.T.);
#8081=ORIENTED_EDGE('',*,*,#6261,.T.);
#8082=ORIENTED_EDGE('',*,*,#6262,.T.);
#8083=ORIENTED_EDGE('',*,*,#6263,.T.);
#8084=ORIENTED_EDGE('',*,*,#6264,.T.);
#8085=ORIENTED_EDGE('',*,*,#6265,.T.);
#8086=ORIENTED_EDGE('',*,*,#6266,.T.);
#8087=ORIENTED_EDGE('',*,*,#6267,.T.);
#8088=ORIENTED_EDGE('',*,*,#6268,.T.);
#8089=ORIENTED_EDGE('',*,*,#6257,.F.);
#8090=ORIENTED_EDGE('',*,*,#6002,.F.);
#8091=ORIENTED_EDGE('',*,*,#6269,.T.);
#8092=ORIENTED_EDGE('',*,*,#6270,.T.);
#8093=ORIENTED_EDGE('',*,*,#6271,.T.);
#8094=ORIENTED_EDGE('',*,*,#6272,.T.);
#8095=ORIENTED_EDGE('',*,*,#6269,.F.);
#8096=ORIENTED_EDGE('',*,*,#6016,.F.);
#8097=ORIENTED_EDGE('',*,*,#6271,.F.);
#8098=ORIENTED_EDGE('',*,*,#6015,.F.);
#8099=ORIENTED_EDGE('',*,*,#6273,.T.);
#8100=ORIENTED_EDGE('',*,*,#6274,.T.);
#8101=ORIENTED_EDGE('',*,*,#6275,.T.);
#8102=ORIENTED_EDGE('',*,*,#6276,.T.);
#8103=ORIENTED_EDGE('',*,*,#6277,.T.);
#8104=ORIENTED_EDGE('',*,*,#6278,.T.);
#8105=ORIENTED_EDGE('',*,*,#6273,.F.);
#8106=ORIENTED_EDGE('',*,*,#6014,.F.);
#8107=ORIENTED_EDGE('',*,*,#6279,.T.);
#8108=ORIENTED_EDGE('',*,*,#6280,.T.);
#8109=ORIENTED_EDGE('',*,*,#6281,.T.);
#8110=ORIENTED_EDGE('',*,*,#6282,.T.);
#8111=ORIENTED_EDGE('',*,*,#6283,.T.);
#8112=ORIENTED_EDGE('',*,*,#6284,.T.);
#8113=ORIENTED_EDGE('',*,*,#6285,.T.);
#8114=ORIENTED_EDGE('',*,*,#6286,.T.);
#8115=ORIENTED_EDGE('',*,*,#6279,.F.);
#8116=ORIENTED_EDGE('',*,*,#6013,.F.);
#8117=ORIENTED_EDGE('',*,*,#6287,.T.);
#8118=ORIENTED_EDGE('',*,*,#6288,.T.);
#8119=ORIENTED_EDGE('',*,*,#6289,.T.);
#8120=ORIENTED_EDGE('',*,*,#6290,.T.);
#8121=ORIENTED_EDGE('',*,*,#6291,.T.);
#8122=ORIENTED_EDGE('',*,*,#6292,.T.);
#8123=ORIENTED_EDGE('',*,*,#6287,.F.);
#8124=ORIENTED_EDGE('',*,*,#6012,.F.);
#8125=ORIENTED_EDGE('',*,*,#6291,.F.);
#8126=ORIENTED_EDGE('',*,*,#6011,.F.);
#8127=ORIENTED_EDGE('',*,*,#6293,.T.);
#8128=ORIENTED_EDGE('',*,*,#6294,.T.);
#8129=ORIENTED_EDGE('',*,*,#6295,.T.);
#8130=ORIENTED_EDGE('',*,*,#6296,.T.);
#8131=ORIENTED_EDGE('',*,*,#6293,.F.);
#8132=ORIENTED_EDGE('',*,*,#6010,.F.);
#8133=ORIENTED_EDGE('',*,*,#6297,.T.);
#8134=ORIENTED_EDGE('',*,*,#6298,.T.);
#8135=ORIENTED_EDGE('',*,*,#6299,.T.);
#8136=ORIENTED_EDGE('',*,*,#6300,.T.);
#8137=ORIENTED_EDGE('',*,*,#6301,.T.);
#8138=ORIENTED_EDGE('',*,*,#6302,.T.);
#8139=ORIENTED_EDGE('',*,*,#6303,.T.);
#8140=ORIENTED_EDGE('',*,*,#6304,.T.);
#8141=ORIENTED_EDGE('',*,*,#6305,.T.);
#8142=ORIENTED_EDGE('',*,*,#6306,.T.);
#8143=ORIENTED_EDGE('',*,*,#6307,.T.);
#8144=ORIENTED_EDGE('',*,*,#6308,.T.);
#8145=ORIENTED_EDGE('',*,*,#6297,.F.);
#8146=ORIENTED_EDGE('',*,*,#6009,.F.);
#8147=ORIENTED_EDGE('',*,*,#6021,.F.);
#8148=ORIENTED_EDGE('',*,*,#6309,.T.);
#8149=ORIENTED_EDGE('',*,*,#6249,.F.);
#8150=ORIENTED_EDGE('',*,*,#6004,.F.);
#8151=ORIENTED_EDGE('',*,*,#6256,.F.);
#8152=ORIENTED_EDGE('',*,*,#6310,.T.);
#8153=ORIENTED_EDGE('',*,*,#6311,.F.);
#8154=ORIENTED_EDGE('',*,*,#6312,.F.);
#8155=ORIENTED_EDGE('',*,*,#6313,.F.);
#8156=ORIENTED_EDGE('',*,*,#6019,.F.);
#8157=ORIENTED_EDGE('',*,*,#6024,.F.);
#8158=ORIENTED_EDGE('',*,*,#6314,.F.);
#8159=ORIENTED_EDGE('',*,*,#6040,.F.);
#8160=ORIENTED_EDGE('',*,*,#6315,.F.);
#8161=ORIENTED_EDGE('',*,*,#6311,.T.);
#8162=ORIENTED_EDGE('',*,*,#6023,.F.);
#8163=ORIENTED_EDGE('',*,*,#6026,.T.);
#8164=ORIENTED_EDGE('',*,*,#6041,.F.);
#8165=ORIENTED_EDGE('',*,*,#6314,.T.);
#8166=ORIENTED_EDGE('',*,*,#6028,.F.);
#8167=ORIENTED_EDGE('',*,*,#6316,.T.);
#8168=ORIENTED_EDGE('',*,*,#6317,.T.);
#8169=ORIENTED_EDGE('',*,*,#6318,.T.);
#8170=ORIENTED_EDGE('',*,*,#6319,.F.);
#8171=ORIENTED_EDGE('',*,*,#6320,.F.);
#8172=ORIENTED_EDGE('',*,*,#6316,.F.);
#8173=ORIENTED_EDGE('',*,*,#6027,.F.);
#8174=ORIENTED_EDGE('',*,*,#6321,.F.);
#8175=ORIENTED_EDGE('',*,*,#6322,.F.);
#8176=ORIENTED_EDGE('',*,*,#6323,.T.);
#8177=ORIENTED_EDGE('',*,*,#6321,.T.);
#8178=ORIENTED_EDGE('',*,*,#6064,.F.);
#8179=ORIENTED_EDGE('',*,*,#6324,.T.);
#8180=ORIENTED_EDGE('',*,*,#6325,.T.);
#8181=ORIENTED_EDGE('',*,*,#6324,.F.);
#8182=ORIENTED_EDGE('',*,*,#6063,.F.);
#8183=ORIENTED_EDGE('',*,*,#6326,.T.);
#8184=ORIENTED_EDGE('',*,*,#6327,.T.);
#8185=ORIENTED_EDGE('',*,*,#6328,.T.);
#8186=ORIENTED_EDGE('',*,*,#6329,.F.);
#8187=ORIENTED_EDGE('',*,*,#6326,.F.);
#8188=ORIENTED_EDGE('',*,*,#6062,.F.);
#8189=ORIENTED_EDGE('',*,*,#6330,.F.);
#8190=ORIENTED_EDGE('',*,*,#6330,.T.);
#8191=ORIENTED_EDGE('',*,*,#6061,.F.);
#8192=ORIENTED_EDGE('',*,*,#6107,.F.);
#8193=ORIENTED_EDGE('',*,*,#6113,.F.);
#8194=ORIENTED_EDGE('',*,*,#6111,.T.);
#8195=ORIENTED_EDGE('',*,*,#6108,.F.);
#8196=ORIENTED_EDGE('',*,*,#6060,.F.);
#8197=ORIENTED_EDGE('',*,*,#6331,.T.);
#8198=ORIENTED_EDGE('',*,*,#6332,.T.);
#8199=ORIENTED_EDGE('',*,*,#6333,.T.);
#8200=ORIENTED_EDGE('',*,*,#6115,.T.);
#8201=ORIENTED_EDGE('',*,*,#6334,.T.);
#8202=ORIENTED_EDGE('',*,*,#6331,.F.);
#8203=ORIENTED_EDGE('',*,*,#6059,.F.);
#8204=ORIENTED_EDGE('',*,*,#6335,.T.);
#8205=ORIENTED_EDGE('',*,*,#6057,.F.);
#8206=ORIENTED_EDGE('',*,*,#6336,.F.);
#8207=ORIENTED_EDGE('',*,*,#6337,.F.);
#8208=ORIENTED_EDGE('',*,*,#6338,.F.);
#8209=ORIENTED_EDGE('',*,*,#6339,.F.);
#8210=ORIENTED_EDGE('',*,*,#6340,.F.);
#8211=ORIENTED_EDGE('',*,*,#6336,.T.);
#8212=ORIENTED_EDGE('',*,*,#6056,.F.);
#8213=ORIENTED_EDGE('',*,*,#6341,.F.);
#8214=ORIENTED_EDGE('',*,*,#6339,.T.);
#8215=ORIENTED_EDGE('',*,*,#6055,.F.);
#8216=ORIENTED_EDGE('',*,*,#6342,.F.);
#8217=ORIENTED_EDGE('',*,*,#6343,.T.);
#8218=ORIENTED_EDGE('',*,*,#6344,.T.);
#8219=ORIENTED_EDGE('',*,*,#6053,.F.);
#8220=ORIENTED_EDGE('',*,*,#6345,.T.);
#8221=ORIENTED_EDGE('',*,*,#6117,.T.);
#8222=ORIENTED_EDGE('',*,*,#6346,.T.);
#8223=ORIENTED_EDGE('',*,*,#6347,.T.);
#8224=ORIENTED_EDGE('',*,*,#6345,.F.);
#8225=ORIENTED_EDGE('',*,*,#6052,.F.);
#8226=ORIENTED_EDGE('',*,*,#6348,.T.);
#8227=ORIENTED_EDGE('',*,*,#6349,.T.);
#8228=ORIENTED_EDGE('',*,*,#6350,.F.);
#8229=ORIENTED_EDGE('',*,*,#6351,.T.);
#8230=ORIENTED_EDGE('',*,*,#6051,.F.);
#8231=ORIENTED_EDGE('',*,*,#6352,.T.);
#8232=ORIENTED_EDGE('',*,*,#6121,.T.);
#8233=ORIENTED_EDGE('',*,*,#6353,.T.);
#8234=ORIENTED_EDGE('',*,*,#6354,.T.);
#8235=ORIENTED_EDGE('',*,*,#6050,.F.);
#8236=ORIENTED_EDGE('',*,*,#6355,.F.);
#8237=ORIENTED_EDGE('',*,*,#6122,.T.);
#8238=ORIENTED_EDGE('',*,*,#6352,.F.);
#8239=ORIENTED_EDGE('',*,*,#6049,.F.);
#8240=ORIENTED_EDGE('',*,*,#6355,.T.);
#8241=ORIENTED_EDGE('',*,*,#6048,.F.);
#8242=ORIENTED_EDGE('',*,*,#6356,.T.);
#8243=ORIENTED_EDGE('',*,*,#6123,.T.);
#8244=ORIENTED_EDGE('',*,*,#6357,.F.);
#8245=ORIENTED_EDGE('',*,*,#6124,.T.);
#8246=ORIENTED_EDGE('',*,*,#6356,.F.);
#8247=ORIENTED_EDGE('',*,*,#6047,.F.);
#8248=ORIENTED_EDGE('',*,*,#6357,.T.);
#8249=ORIENTED_EDGE('',*,*,#6046,.F.);
#8250=ORIENTED_EDGE('',*,*,#6358,.T.);
#8251=ORIENTED_EDGE('',*,*,#6359,.T.);
#8252=ORIENTED_EDGE('',*,*,#6125,.T.);
#8253=ORIENTED_EDGE('',*,*,#6360,.F.);
#8254=ORIENTED_EDGE('',*,*,#6361,.T.);
#8255=ORIENTED_EDGE('',*,*,#6045,.F.);
#8256=ORIENTED_EDGE('',*,*,#6362,.T.);
#8257=ORIENTED_EDGE('',*,*,#6069,.T.);
#8258=ORIENTED_EDGE('',*,*,#6363,.T.);
#8259=ORIENTED_EDGE('',*,*,#6364,.T.);
#8260=ORIENTED_EDGE('',*,*,#6044,.F.);
#8261=ORIENTED_EDGE('',*,*,#6066,.F.);
#8262=ORIENTED_EDGE('',*,*,#6070,.T.);
#8263=ORIENTED_EDGE('',*,*,#6362,.F.);
#8264=ORIENTED_EDGE('',*,*,#6043,.F.);
#8265=ORIENTED_EDGE('',*,*,#6365,.T.);
#8266=ORIENTED_EDGE('',*,*,#6366,.F.);
#8267=ORIENTED_EDGE('',*,*,#6039,.F.);
#8268=ORIENTED_EDGE('',*,*,#6038,.F.);
#8269=ORIENTED_EDGE('',*,*,#6367,.F.);
#8270=ORIENTED_EDGE('',*,*,#6300,.F.);
#8271=ORIENTED_EDGE('',*,*,#6368,.F.);
#8272=ORIENTED_EDGE('',*,*,#6369,.F.);
#8273=ORIENTED_EDGE('',*,*,#6301,.F.);
#8274=ORIENTED_EDGE('',*,*,#6367,.T.);
#8275=ORIENTED_EDGE('',*,*,#6037,.F.);
#8276=ORIENTED_EDGE('',*,*,#6370,.T.);
#8277=ORIENTED_EDGE('',*,*,#6036,.F.);
#8278=ORIENTED_EDGE('',*,*,#6371,.F.);
#8279=ORIENTED_EDGE('',*,*,#6302,.F.);
#8280=ORIENTED_EDGE('',*,*,#6370,.F.);
#8281=ORIENTED_EDGE('',*,*,#6303,.F.);
#8282=ORIENTED_EDGE('',*,*,#6371,.T.);
#8283=ORIENTED_EDGE('',*,*,#6035,.F.);
#8284=ORIENTED_EDGE('',*,*,#6372,.T.);
#8285=ORIENTED_EDGE('',*,*,#6304,.F.);
#8286=ORIENTED_EDGE('',*,*,#6372,.F.);
#8287=ORIENTED_EDGE('',*,*,#6034,.F.);
#8288=ORIENTED_EDGE('',*,*,#6373,.F.);
#8289=ORIENTED_EDGE('',*,*,#6374,.F.);
#8290=ORIENTED_EDGE('',*,*,#6375,.T.);
#8291=ORIENTED_EDGE('',*,*,#6376,.F.);
#8292=ORIENTED_EDGE('',*,*,#6033,.F.);
#8293=ORIENTED_EDGE('',*,*,#6032,.F.);
#8294=ORIENTED_EDGE('',*,*,#6377,.F.);
#8295=ORIENTED_EDGE('',*,*,#6308,.F.);
#8296=ORIENTED_EDGE('',*,*,#6378,.F.);
#8297=ORIENTED_EDGE('',*,*,#6379,.F.);
#8298=ORIENTED_EDGE('',*,*,#6295,.F.);
#8299=ORIENTED_EDGE('',*,*,#6377,.T.);
#8300=ORIENTED_EDGE('',*,*,#6031,.F.);
#8301=ORIENTED_EDGE('',*,*,#6380,.T.);
#8302=ORIENTED_EDGE('',*,*,#6292,.F.);
#8303=ORIENTED_EDGE('',*,*,#6294,.F.);
#8304=ORIENTED_EDGE('',*,*,#6296,.F.);
#8305=ORIENTED_EDGE('',*,*,#6380,.F.);
#8306=ORIENTED_EDGE('',*,*,#6030,.F.);
#8307=ORIENTED_EDGE('',*,*,#6288,.F.);
#8308=ORIENTED_EDGE('',*,*,#6289,.F.);
#8309=ORIENTED_EDGE('',*,*,#6029,.F.);
#8310=ORIENTED_EDGE('',*,*,#6318,.F.);
#8311=ORIENTED_EDGE('',*,*,#6381,.T.);
#8312=ORIENTED_EDGE('',*,*,#6363,.F.);
#8313=ORIENTED_EDGE('',*,*,#6068,.T.);
#8314=ORIENTED_EDGE('',*,*,#6382,.T.);
#8315=ORIENTED_EDGE('',*,*,#6094,.F.);
#8316=ORIENTED_EDGE('',*,*,#6383,.F.);
#8317=ORIENTED_EDGE('',*,*,#6384,.F.);
#8318=ORIENTED_EDGE('',*,*,#6385,.F.);
#8319=ORIENTED_EDGE('',*,*,#6386,.F.);
#8320=ORIENTED_EDGE('',*,*,#6097,.T.);
#8321=ORIENTED_EDGE('',*,*,#5831,.T.);
#8322=ORIENTED_EDGE('',*,*,#6387,.F.);
#8323=ORIENTED_EDGE('',*,*,#6388,.F.);
#8324=ORIENTED_EDGE('',*,*,#6389,.F.);
#8325=ORIENTED_EDGE('',*,*,#6390,.F.);
#8326=ORIENTED_EDGE('',*,*,#6083,.T.);
#8327=ORIENTED_EDGE('',*,*,#5834,.T.);
#8328=ORIENTED_EDGE('',*,*,#6191,.T.);
#8329=ORIENTED_EDGE('',*,*,#6391,.F.);
#8330=ORIENTED_EDGE('',*,*,#6392,.F.);
#8331=ORIENTED_EDGE('',*,*,#6393,.F.);
#8332=ORIENTED_EDGE('',*,*,#6394,.F.);
#8333=ORIENTED_EDGE('',*,*,#6075,.T.);
#8334=ORIENTED_EDGE('',*,*,#6073,.F.);
#8335=ORIENTED_EDGE('',*,*,#5837,.T.);
#8336=ORIENTED_EDGE('',*,*,#6105,.T.);
#8337=ORIENTED_EDGE('',*,*,#6395,.F.);
#8338=ORIENTED_EDGE('',*,*,#6396,.F.);
#8339=ORIENTED_EDGE('',*,*,#6397,.F.);
#8340=ORIENTED_EDGE('',*,*,#6398,.F.);
#8341=ORIENTED_EDGE('',*,*,#6110,.F.);
#8342=ORIENTED_EDGE('',*,*,#5840,.T.);
#8343=ORIENTED_EDGE('',*,*,#6399,.F.);
#8344=ORIENTED_EDGE('',*,*,#6400,.F.);
#8345=ORIENTED_EDGE('',*,*,#6401,.F.);
#8346=ORIENTED_EDGE('',*,*,#6402,.F.);
#8347=ORIENTED_EDGE('',*,*,#6119,.T.);
#8348=ORIENTED_EDGE('',*,*,#5843,.T.);
#8349=ORIENTED_EDGE('',*,*,#6127,.T.);
#8350=ORIENTED_EDGE('',*,*,#6403,.F.);
#8351=ORIENTED_EDGE('',*,*,#6404,.F.);
#8352=ORIENTED_EDGE('',*,*,#6405,.F.);
#8353=ORIENTED_EDGE('',*,*,#6382,.F.);
#8354=ORIENTED_EDGE('',*,*,#6067,.F.);
#8355=ORIENTED_EDGE('',*,*,#6129,.F.);
#8356=ORIENTED_EDGE('',*,*,#5846,.T.);
#8357=ORIENTED_EDGE('',*,*,#6406,.T.);
#8358=ORIENTED_EDGE('',*,*,#6407,.T.);
#8359=ORIENTED_EDGE('',*,*,#6076,.T.);
#8360=ORIENTED_EDGE('',*,*,#6394,.T.);
#8361=ORIENTED_EDGE('',*,*,#6408,.F.);
#8362=ORIENTED_EDGE('',*,*,#6078,.T.);
#8363=ORIENTED_EDGE('',*,*,#6409,.F.);
#8364=ORIENTED_EDGE('',*,*,#6234,.F.);
#8365=ORIENTED_EDGE('',*,*,#6410,.T.);
#8366=ORIENTED_EDGE('',*,*,#6079,.T.);
#8367=ORIENTED_EDGE('',*,*,#6408,.T.);
#8368=ORIENTED_EDGE('',*,*,#6233,.F.);
#8369=ORIENTED_EDGE('',*,*,#6411,.F.);
#8370=ORIENTED_EDGE('',*,*,#6080,.T.);
#8371=ORIENTED_EDGE('',*,*,#6410,.F.);
#8372=ORIENTED_EDGE('',*,*,#6232,.F.);
#8373=ORIENTED_EDGE('',*,*,#6412,.T.);
#8374=ORIENTED_EDGE('',*,*,#6387,.T.);
#8375=ORIENTED_EDGE('',*,*,#6082,.T.);
#8376=ORIENTED_EDGE('',*,*,#6413,.T.);
#8377=ORIENTED_EDGE('',*,*,#6414,.T.);
#8378=ORIENTED_EDGE('',*,*,#6415,.T.);
#8379=ORIENTED_EDGE('',*,*,#6084,.T.);
#8380=ORIENTED_EDGE('',*,*,#6390,.T.);
#8381=ORIENTED_EDGE('',*,*,#6416,.F.);
#8382=ORIENTED_EDGE('',*,*,#6086,.T.);
#8383=ORIENTED_EDGE('',*,*,#6417,.F.);
#8384=ORIENTED_EDGE('',*,*,#6418,.F.);
#8385=ORIENTED_EDGE('',*,*,#6096,.F.);
#8386=ORIENTED_EDGE('',*,*,#6091,.T.);
#8387=ORIENTED_EDGE('',*,*,#6089,.F.);
#8388=ORIENTED_EDGE('',*,*,#6087,.T.);
#8389=ORIENTED_EDGE('',*,*,#6416,.T.);
#8390=ORIENTED_EDGE('',*,*,#6419,.T.);
#8391=ORIENTED_EDGE('',*,*,#6420,.T.);
#8392=ORIENTED_EDGE('',*,*,#6221,.F.);
#8393=ORIENTED_EDGE('',*,*,#6093,.F.);
#8394=ORIENTED_EDGE('',*,*,#6220,.F.);
#8395=ORIENTED_EDGE('',*,*,#6421,.F.);
#8396=ORIENTED_EDGE('',*,*,#6422,.T.);
#8397=ORIENTED_EDGE('',*,*,#6423,.T.);
#8398=ORIENTED_EDGE('',*,*,#6098,.T.);
#8399=ORIENTED_EDGE('',*,*,#6386,.T.);
#8400=ORIENTED_EDGE('',*,*,#6424,.F.);
#8401=ORIENTED_EDGE('',*,*,#6100,.T.);
#8402=ORIENTED_EDGE('',*,*,#6425,.F.);
#8403=ORIENTED_EDGE('',*,*,#6426,.F.);
#8404=ORIENTED_EDGE('',*,*,#6427,.T.);
#8405=ORIENTED_EDGE('',*,*,#6101,.T.);
#8406=ORIENTED_EDGE('',*,*,#6424,.T.);
#8407=ORIENTED_EDGE('',*,*,#6428,.T.);
#8408=ORIENTED_EDGE('',*,*,#6429,.F.);
#8409=ORIENTED_EDGE('',*,*,#6102,.T.);
#8410=ORIENTED_EDGE('',*,*,#6427,.F.);
#8411=ORIENTED_EDGE('',*,*,#6430,.F.);
#8412=ORIENTED_EDGE('',*,*,#6431,.T.);
#8413=ORIENTED_EDGE('',*,*,#6395,.T.);
#8414=ORIENTED_EDGE('',*,*,#6104,.T.);
#8415=ORIENTED_EDGE('',*,*,#6432,.T.);
#8416=ORIENTED_EDGE('',*,*,#6346,.F.);
#8417=ORIENTED_EDGE('',*,*,#6116,.T.);
#8418=ORIENTED_EDGE('',*,*,#6333,.F.);
#8419=ORIENTED_EDGE('',*,*,#6433,.F.);
#8420=ORIENTED_EDGE('',*,*,#6434,.T.);
#8421=ORIENTED_EDGE('',*,*,#6399,.T.);
#8422=ORIENTED_EDGE('',*,*,#6118,.T.);
#8423=ORIENTED_EDGE('',*,*,#6349,.F.);
#8424=ORIENTED_EDGE('',*,*,#6435,.T.);
#8425=ORIENTED_EDGE('',*,*,#6353,.F.);
#8426=ORIENTED_EDGE('',*,*,#6120,.T.);
#8427=ORIENTED_EDGE('',*,*,#6402,.T.);
#8428=ORIENTED_EDGE('',*,*,#6436,.T.);
#8429=ORIENTED_EDGE('',*,*,#6403,.T.);
#8430=ORIENTED_EDGE('',*,*,#6126,.T.);
#8431=ORIENTED_EDGE('',*,*,#6359,.F.);
#8432=ORIENTED_EDGE('',*,*,#6132,.T.);
#8433=ORIENTED_EDGE('',*,*,#6130,.F.);
#8434=ORIENTED_EDGE('',*,*,#6205,.T.);
#8435=ORIENTED_EDGE('',*,*,#6437,.T.);
#8436=ORIENTED_EDGE('',*,*,#6135,.T.);
#8437=ORIENTED_EDGE('',*,*,#6437,.F.);
#8438=ORIENTED_EDGE('',*,*,#6204,.T.);
#8439=ORIENTED_EDGE('',*,*,#6438,.T.);
#8440=ORIENTED_EDGE('',*,*,#6138,.T.);
#8441=ORIENTED_EDGE('',*,*,#6438,.F.);
#8442=ORIENTED_EDGE('',*,*,#6203,.T.);
#8443=ORIENTED_EDGE('',*,*,#6439,.T.);
#8444=ORIENTED_EDGE('',*,*,#6142,.F.);
#8445=ORIENTED_EDGE('',*,*,#6440,.T.);
#8446=ORIENTED_EDGE('',*,*,#6202,.T.);
#8447=ORIENTED_EDGE('',*,*,#6441,.T.);
#8448=ORIENTED_EDGE('',*,*,#6201,.T.);
#8449=ORIENTED_EDGE('',*,*,#6442,.T.);
#8450=ORIENTED_EDGE('',*,*,#6149,.T.);
#8451=ORIENTED_EDGE('',*,*,#6443,.T.);
#8452=ORIENTED_EDGE('',*,*,#6151,.T.);
#8453=ORIENTED_EDGE('',*,*,#6442,.F.);
#8454=ORIENTED_EDGE('',*,*,#6200,.T.);
#8455=ORIENTED_EDGE('',*,*,#6444,.T.);
#8456=ORIENTED_EDGE('',*,*,#6154,.T.);
#8457=ORIENTED_EDGE('',*,*,#6444,.F.);
#8458=ORIENTED_EDGE('',*,*,#6199,.T.);
#8459=ORIENTED_EDGE('',*,*,#6445,.T.);
#8460=ORIENTED_EDGE('',*,*,#6158,.F.);
#8461=ORIENTED_EDGE('',*,*,#6446,.T.);
#8462=ORIENTED_EDGE('',*,*,#6198,.T.);
#8463=ORIENTED_EDGE('',*,*,#6447,.T.);
#8464=ORIENTED_EDGE('',*,*,#6197,.T.);
#8465=ORIENTED_EDGE('',*,*,#6448,.T.);
#8466=ORIENTED_EDGE('',*,*,#6165,.T.);
#8467=ORIENTED_EDGE('',*,*,#6449,.T.);
#8468=ORIENTED_EDGE('',*,*,#6167,.T.);
#8469=ORIENTED_EDGE('',*,*,#6448,.F.);
#8470=ORIENTED_EDGE('',*,*,#6196,.T.);
#8471=ORIENTED_EDGE('',*,*,#6450,.T.);
#8472=ORIENTED_EDGE('',*,*,#6170,.T.);
#8473=ORIENTED_EDGE('',*,*,#6450,.F.);
#8474=ORIENTED_EDGE('',*,*,#6195,.T.);
#8475=ORIENTED_EDGE('',*,*,#6451,.T.);
#8476=ORIENTED_EDGE('',*,*,#6174,.F.);
#8477=ORIENTED_EDGE('',*,*,#6452,.T.);
#8478=ORIENTED_EDGE('',*,*,#6194,.T.);
#8479=ORIENTED_EDGE('',*,*,#6453,.T.);
#8480=ORIENTED_EDGE('',*,*,#6193,.T.);
#8481=ORIENTED_EDGE('',*,*,#6454,.T.);
#8482=ORIENTED_EDGE('',*,*,#6181,.T.);
#8483=ORIENTED_EDGE('',*,*,#6455,.T.);
#8484=ORIENTED_EDGE('',*,*,#6183,.T.);
#8485=ORIENTED_EDGE('',*,*,#6454,.F.);
#8486=ORIENTED_EDGE('',*,*,#6192,.T.);
#8487=ORIENTED_EDGE('',*,*,#6456,.T.);
#8488=ORIENTED_EDGE('',*,*,#6184,.T.);
#8489=ORIENTED_EDGE('',*,*,#6456,.F.);
#8490=ORIENTED_EDGE('',*,*,#6206,.T.);
#8491=ORIENTED_EDGE('',*,*,#6186,.F.);
#8492=ORIENTED_EDGE('',*,*,#6457,.F.);
#8493=ORIENTED_EDGE('',*,*,#6188,.T.);
#8494=ORIENTED_EDGE('',*,*,#6207,.F.);
#8495=ORIENTED_EDGE('',*,*,#6238,.F.);
#8496=ORIENTED_EDGE('',*,*,#6457,.T.);
#8497=ORIENTED_EDGE('',*,*,#6237,.F.);
#8498=ORIENTED_EDGE('',*,*,#6458,.T.);
#8499=ORIENTED_EDGE('',*,*,#6459,.T.);
#8500=ORIENTED_EDGE('',*,*,#6189,.T.);
#8501=ORIENTED_EDGE('',*,*,#6460,.T.);
#8502=ORIENTED_EDGE('',*,*,#6391,.T.);
#8503=ORIENTED_EDGE('',*,*,#6190,.T.);
#8504=ORIENTED_EDGE('',*,*,#6459,.F.);
#8505=ORIENTED_EDGE('',*,*,#6253,.F.);
#8506=ORIENTED_EDGE('',*,*,#6461,.T.);
#8507=ORIENTED_EDGE('',*,*,#6239,.F.);
#8508=ORIENTED_EDGE('',*,*,#6210,.T.);
#8509=ORIENTED_EDGE('',*,*,#6272,.F.);
#8510=ORIENTED_EDGE('',*,*,#6276,.F.);
#8511=ORIENTED_EDGE('',*,*,#6213,.F.);
#8512=ORIENTED_EDGE('',*,*,#6462,.F.);
#8513=ORIENTED_EDGE('',*,*,#6258,.F.);
#8514=ORIENTED_EDGE('',*,*,#6270,.F.);
#8515=ORIENTED_EDGE('',*,*,#6259,.F.);
#8516=ORIENTED_EDGE('',*,*,#6462,.T.);
#8517=ORIENTED_EDGE('',*,*,#6212,.F.);
#8518=ORIENTED_EDGE('',*,*,#6463,.T.);
#8519=ORIENTED_EDGE('',*,*,#6260,.F.);
#8520=ORIENTED_EDGE('',*,*,#6463,.F.);
#8521=ORIENTED_EDGE('',*,*,#6248,.F.);
#8522=ORIENTED_EDGE('',*,*,#6464,.F.);
#8523=ORIENTED_EDGE('',*,*,#6465,.F.);
#8524=ORIENTED_EDGE('',*,*,#6466,.T.);
#8525=ORIENTED_EDGE('',*,*,#6467,.F.);
#8526=ORIENTED_EDGE('',*,*,#6247,.F.);
#8527=ORIENTED_EDGE('',*,*,#6246,.F.);
#8528=ORIENTED_EDGE('',*,*,#6468,.F.);
#8529=ORIENTED_EDGE('',*,*,#6264,.F.);
#8530=ORIENTED_EDGE('',*,*,#6469,.F.);
#8531=ORIENTED_EDGE('',*,*,#6470,.F.);
#8532=ORIENTED_EDGE('',*,*,#6265,.F.);
#8533=ORIENTED_EDGE('',*,*,#6468,.T.);
#8534=ORIENTED_EDGE('',*,*,#6245,.F.);
#8535=ORIENTED_EDGE('',*,*,#6471,.T.);
#8536=ORIENTED_EDGE('',*,*,#6266,.F.);
#8537=ORIENTED_EDGE('',*,*,#6471,.F.);
#8538=ORIENTED_EDGE('',*,*,#6244,.F.);
#8539=ORIENTED_EDGE('',*,*,#6472,.F.);
#8540=ORIENTED_EDGE('',*,*,#6267,.F.);
#8541=ORIENTED_EDGE('',*,*,#6472,.T.);
#8542=ORIENTED_EDGE('',*,*,#6243,.F.);
#8543=ORIENTED_EDGE('',*,*,#6473,.T.);
#8544=ORIENTED_EDGE('',*,*,#6268,.F.);
#8545=ORIENTED_EDGE('',*,*,#6473,.F.);
#8546=ORIENTED_EDGE('',*,*,#6242,.F.);
#8547=ORIENTED_EDGE('',*,*,#6474,.F.);
#8548=ORIENTED_EDGE('',*,*,#6475,.F.);
#8549=ORIENTED_EDGE('',*,*,#6476,.T.);
#8550=ORIENTED_EDGE('',*,*,#6477,.F.);
#8551=ORIENTED_EDGE('',*,*,#6241,.F.);
#8552=ORIENTED_EDGE('',*,*,#6240,.F.);
#8553=ORIENTED_EDGE('',*,*,#6461,.F.);
#8554=ORIENTED_EDGE('',*,*,#6252,.F.);
#8555=ORIENTED_EDGE('',*,*,#6478,.F.);
#8556=ORIENTED_EDGE('',*,*,#6479,.F.);
#8557=ORIENTED_EDGE('',*,*,#6480,.T.);
#8558=ORIENTED_EDGE('',*,*,#6481,.T.);
#8559=ORIENTED_EDGE('',*,*,#6236,.F.);
#8560=ORIENTED_EDGE('',*,*,#6409,.T.);
#8561=ORIENTED_EDGE('',*,*,#6077,.T.);
#8562=ORIENTED_EDGE('',*,*,#6407,.F.);
#8563=ORIENTED_EDGE('',*,*,#6482,.T.);
#8564=ORIENTED_EDGE('',*,*,#6235,.F.);
#8565=ORIENTED_EDGE('',*,*,#6411,.T.);
#8566=ORIENTED_EDGE('',*,*,#6231,.F.);
#8567=ORIENTED_EDGE('',*,*,#6483,.T.);
#8568=ORIENTED_EDGE('',*,*,#6413,.F.);
#8569=ORIENTED_EDGE('',*,*,#6081,.T.);
#8570=ORIENTED_EDGE('',*,*,#6484,.T.);
#8571=ORIENTED_EDGE('',*,*,#6485,.T.);
#8572=ORIENTED_EDGE('',*,*,#6230,.F.);
#8573=ORIENTED_EDGE('',*,*,#6486,.T.);
#8574=ORIENTED_EDGE('',*,*,#6229,.F.);
#8575=ORIENTED_EDGE('',*,*,#6487,.T.);
#8576=ORIENTED_EDGE('',*,*,#6488,.T.);
#8577=ORIENTED_EDGE('',*,*,#6417,.T.);
#8578=ORIENTED_EDGE('',*,*,#6085,.T.);
#8579=ORIENTED_EDGE('',*,*,#6415,.F.);
#8580=ORIENTED_EDGE('',*,*,#6489,.T.);
#8581=ORIENTED_EDGE('',*,*,#6487,.F.);
#8582=ORIENTED_EDGE('',*,*,#6228,.F.);
#8583=ORIENTED_EDGE('',*,*,#6490,.T.);
#8584=ORIENTED_EDGE('',*,*,#6226,.F.);
#8585=ORIENTED_EDGE('',*,*,#6491,.F.);
#8586=ORIENTED_EDGE('',*,*,#6492,.F.);
#8587=ORIENTED_EDGE('',*,*,#6493,.F.);
#8588=ORIENTED_EDGE('',*,*,#6494,.F.);
#8589=ORIENTED_EDGE('',*,*,#6495,.F.);
#8590=ORIENTED_EDGE('',*,*,#6491,.T.);
#8591=ORIENTED_EDGE('',*,*,#6225,.F.);
#8592=ORIENTED_EDGE('',*,*,#6496,.F.);
#8593=ORIENTED_EDGE('',*,*,#6494,.T.);
#8594=ORIENTED_EDGE('',*,*,#6224,.F.);
#8595=ORIENTED_EDGE('',*,*,#6497,.F.);
#8596=ORIENTED_EDGE('',*,*,#6498,.T.);
#8597=ORIENTED_EDGE('',*,*,#6499,.T.);
#8598=ORIENTED_EDGE('',*,*,#6222,.F.);
#8599=ORIENTED_EDGE('',*,*,#6420,.F.);
#8600=ORIENTED_EDGE('',*,*,#6421,.T.);
#8601=ORIENTED_EDGE('',*,*,#6219,.F.);
#8602=ORIENTED_EDGE('',*,*,#6500,.F.);
#8603=ORIENTED_EDGE('',*,*,#6501,.F.);
#8604=ORIENTED_EDGE('',*,*,#6218,.F.);
#8605=ORIENTED_EDGE('',*,*,#6502,.T.);
#8606=ORIENTED_EDGE('',*,*,#6503,.T.);
#8607=ORIENTED_EDGE('',*,*,#6504,.T.);
#8608=ORIENTED_EDGE('',*,*,#6505,.T.);
#8609=ORIENTED_EDGE('',*,*,#6500,.T.);
#8610=ORIENTED_EDGE('',*,*,#6217,.F.);
#8611=ORIENTED_EDGE('',*,*,#6506,.T.);
#8612=ORIENTED_EDGE('',*,*,#6507,.T.);
#8613=ORIENTED_EDGE('',*,*,#6502,.F.);
#8614=ORIENTED_EDGE('',*,*,#6508,.F.);
#8615=ORIENTED_EDGE('',*,*,#6509,.F.);
#8616=ORIENTED_EDGE('',*,*,#6510,.F.);
#8617=ORIENTED_EDGE('',*,*,#6511,.F.);
#8618=ORIENTED_EDGE('',*,*,#6506,.F.);
#8619=ORIENTED_EDGE('',*,*,#6216,.F.);
#8620=ORIENTED_EDGE('',*,*,#6508,.T.);
#8621=ORIENTED_EDGE('',*,*,#6215,.F.);
#8622=ORIENTED_EDGE('',*,*,#6512,.T.);
#8623=ORIENTED_EDGE('',*,*,#6513,.T.);
#8624=ORIENTED_EDGE('',*,*,#6512,.F.);
#8625=ORIENTED_EDGE('',*,*,#6214,.F.);
#8626=ORIENTED_EDGE('',*,*,#6275,.F.);
#8627=ORIENTED_EDGE('',*,*,#6514,.F.);
#8628=ORIENTED_EDGE('',*,*,#6515,.F.);
#8629=ORIENTED_EDGE('',*,*,#6478,.T.);
#8630=ORIENTED_EDGE('',*,*,#6251,.F.);
#8631=ORIENTED_EDGE('',*,*,#6516,.T.);
#8632=ORIENTED_EDGE('',*,*,#6274,.F.);
#8633=ORIENTED_EDGE('',*,*,#6278,.F.);
#8634=ORIENTED_EDGE('',*,*,#6517,.T.);
#8635=ORIENTED_EDGE('',*,*,#6518,.T.);
#8636=ORIENTED_EDGE('',*,*,#6519,.T.);
#8637=ORIENTED_EDGE('',*,*,#5851,.T.);
#8638=ORIENTED_EDGE('',*,*,#6520,.T.);
#8639=ORIENTED_EDGE('',*,*,#6521,.T.);
#8640=ORIENTED_EDGE('',*,*,#6262,.F.);
#8641=ORIENTED_EDGE('',*,*,#6522,.T.);
#8642=ORIENTED_EDGE('',*,*,#6523,.T.);
#8643=ORIENTED_EDGE('',*,*,#5854,.T.);
#8644=ORIENTED_EDGE('',*,*,#6514,.T.);
#8645=ORIENTED_EDGE('',*,*,#6250,.T.);
#8646=ORIENTED_EDGE('',*,*,#6310,.F.);
#8647=ORIENTED_EDGE('',*,*,#6255,.F.);
#8648=ORIENTED_EDGE('',*,*,#6524,.T.);
#8649=ORIENTED_EDGE('',*,*,#6525,.T.);
#8650=ORIENTED_EDGE('',*,*,#6526,.T.);
#8651=ORIENTED_EDGE('',*,*,#5857,.T.);
#8652=ORIENTED_EDGE('',*,*,#6527,.T.);
#8653=ORIENTED_EDGE('',*,*,#6280,.F.);
#8654=ORIENTED_EDGE('',*,*,#6290,.F.);
#8655=ORIENTED_EDGE('',*,*,#6528,.T.);
#8656=ORIENTED_EDGE('',*,*,#6529,.T.);
#8657=ORIENTED_EDGE('',*,*,#6530,.T.);
#8658=ORIENTED_EDGE('',*,*,#5860,.T.);
#8659=ORIENTED_EDGE('',*,*,#6531,.T.);
#8660=ORIENTED_EDGE('',*,*,#6532,.T.);
#8661=ORIENTED_EDGE('',*,*,#6306,.F.);
#8662=ORIENTED_EDGE('',*,*,#6533,.T.);
#8663=ORIENTED_EDGE('',*,*,#6534,.T.);
#8664=ORIENTED_EDGE('',*,*,#5863,.T.);
#8665=ORIENTED_EDGE('',*,*,#6535,.T.);
#8666=ORIENTED_EDGE('',*,*,#6298,.F.);
#8667=ORIENTED_EDGE('',*,*,#6309,.F.);
#8668=ORIENTED_EDGE('',*,*,#6020,.T.);
#8669=ORIENTED_EDGE('',*,*,#6313,.T.);
#8670=ORIENTED_EDGE('',*,*,#6536,.T.);
#8671=ORIENTED_EDGE('',*,*,#6537,.T.);
#8672=ORIENTED_EDGE('',*,*,#5866,.T.);
#8673=ORIENTED_EDGE('',*,*,#6475,.T.);
#8674=ORIENTED_EDGE('',*,*,#6538,.F.);
#8675=ORIENTED_EDGE('',*,*,#6524,.F.);
#8676=ORIENTED_EDGE('',*,*,#6254,.F.);
#8677=ORIENTED_EDGE('',*,*,#6521,.F.);
#8678=ORIENTED_EDGE('',*,*,#6539,.F.);
#8679=ORIENTED_EDGE('',*,*,#6469,.T.);
#8680=ORIENTED_EDGE('',*,*,#6263,.F.);
#8681=ORIENTED_EDGE('',*,*,#6465,.T.);
#8682=ORIENTED_EDGE('',*,*,#6540,.F.);
#8683=ORIENTED_EDGE('',*,*,#6522,.F.);
#8684=ORIENTED_EDGE('',*,*,#6261,.F.);
#8685=ORIENTED_EDGE('',*,*,#6541,.F.);
#8686=ORIENTED_EDGE('',*,*,#6542,.F.);
#8687=ORIENTED_EDGE('',*,*,#6517,.F.);
#8688=ORIENTED_EDGE('',*,*,#6277,.F.);
#8689=ORIENTED_EDGE('',*,*,#6285,.F.);
#8690=ORIENTED_EDGE('',*,*,#6543,.T.);
#8691=ORIENTED_EDGE('',*,*,#6544,.T.);
#8692=ORIENTED_EDGE('',*,*,#6545,.T.);
#8693=ORIENTED_EDGE('',*,*,#6284,.F.);
#8694=ORIENTED_EDGE('',*,*,#6546,.F.);
#8695=ORIENTED_EDGE('',*,*,#6547,.F.);
#8696=ORIENTED_EDGE('',*,*,#6543,.F.);
#8697=ORIENTED_EDGE('',*,*,#6283,.F.);
#8698=ORIENTED_EDGE('',*,*,#6548,.T.);
#8699=ORIENTED_EDGE('',*,*,#6549,.T.);
#8700=ORIENTED_EDGE('',*,*,#6546,.T.);
#8701=ORIENTED_EDGE('',*,*,#6527,.F.);
#8702=ORIENTED_EDGE('',*,*,#6550,.F.);
#8703=ORIENTED_EDGE('',*,*,#6551,.F.);
#8704=ORIENTED_EDGE('',*,*,#6281,.F.);
#8705=ORIENTED_EDGE('',*,*,#6532,.F.);
#8706=ORIENTED_EDGE('',*,*,#6552,.F.);
#8707=ORIENTED_EDGE('',*,*,#6378,.T.);
#8708=ORIENTED_EDGE('',*,*,#6307,.F.);
#8709=ORIENTED_EDGE('',*,*,#6374,.T.);
#8710=ORIENTED_EDGE('',*,*,#6553,.F.);
#8711=ORIENTED_EDGE('',*,*,#6533,.F.);
#8712=ORIENTED_EDGE('',*,*,#6305,.F.);
#8713=ORIENTED_EDGE('',*,*,#6535,.F.);
#8714=ORIENTED_EDGE('',*,*,#6554,.F.);
#8715=ORIENTED_EDGE('',*,*,#6368,.T.);
#8716=ORIENTED_EDGE('',*,*,#6299,.F.);
#8717=ORIENTED_EDGE('',*,*,#5869,.F.);
#8718=ORIENTED_EDGE('',*,*,#5873,.F.);
#8719=ORIENTED_EDGE('',*,*,#6366,.T.);
#8720=ORIENTED_EDGE('',*,*,#6555,.F.);
#8721=ORIENTED_EDGE('',*,*,#6536,.F.);
#8722=ORIENTED_EDGE('',*,*,#6312,.T.);
#8723=ORIENTED_EDGE('',*,*,#6315,.T.);
#8724=ORIENTED_EDGE('',*,*,#6320,.T.);
#8725=ORIENTED_EDGE('',*,*,#6556,.F.);
#8726=ORIENTED_EDGE('',*,*,#6528,.F.);
#8727=ORIENTED_EDGE('',*,*,#6317,.F.);
#8728=ORIENTED_EDGE('',*,*,#6557,.F.);
#8729=ORIENTED_EDGE('',*,*,#6558,.F.);
#8730=ORIENTED_EDGE('',*,*,#6529,.F.);
#8731=ORIENTED_EDGE('',*,*,#6556,.T.);
#8732=ORIENTED_EDGE('',*,*,#6319,.T.);
#8733=ORIENTED_EDGE('',*,*,#6559,.T.);
#8734=ORIENTED_EDGE('',*,*,#6503,.F.);
#8735=ORIENTED_EDGE('',*,*,#6507,.F.);
#8736=ORIENTED_EDGE('',*,*,#6511,.T.);
#8737=ORIENTED_EDGE('',*,*,#6560,.T.);
#8738=ORIENTED_EDGE('',*,*,#6561,.T.);
#8739=ORIENTED_EDGE('',*,*,#6544,.F.);
#8740=ORIENTED_EDGE('',*,*,#6547,.T.);
#8741=ORIENTED_EDGE('',*,*,#6549,.F.);
#8742=ORIENTED_EDGE('',*,*,#6562,.T.);
#8743=ORIENTED_EDGE('',*,*,#6563,.T.);
#8744=ORIENTED_EDGE('',*,*,#6322,.T.);
#8745=ORIENTED_EDGE('',*,*,#6323,.F.);
#8746=ORIENTED_EDGE('',*,*,#6325,.F.);
#8747=ORIENTED_EDGE('',*,*,#6564,.T.);
#8748=ORIENTED_EDGE('',*,*,#6565,.T.);
#8749=ORIENTED_EDGE('',*,*,#6430,.T.);
#8750=ORIENTED_EDGE('',*,*,#6428,.F.);
#8751=ORIENTED_EDGE('',*,*,#6426,.T.);
#8752=ORIENTED_EDGE('',*,*,#6566,.T.);
#8753=ORIENTED_EDGE('',*,*,#6567,.T.);
#8754=ORIENTED_EDGE('',*,*,#6568,.T.);
#8755=ORIENTED_EDGE('',*,*,#6328,.F.);
#8756=ORIENTED_EDGE('',*,*,#6569,.T.);
#8757=ORIENTED_EDGE('',*,*,#6397,.T.);
#8758=ORIENTED_EDGE('',*,*,#6569,.F.);
#8759=ORIENTED_EDGE('',*,*,#6327,.F.);
#8760=ORIENTED_EDGE('',*,*,#6329,.T.);
#8761=ORIENTED_EDGE('',*,*,#6398,.T.);
#8762=ORIENTED_EDGE('',*,*,#6347,.F.);
#8763=ORIENTED_EDGE('',*,*,#6433,.T.);
#8764=ORIENTED_EDGE('',*,*,#6332,.F.);
#8765=ORIENTED_EDGE('',*,*,#6334,.F.);
#8766=ORIENTED_EDGE('',*,*,#6570,.T.);
#8767=ORIENTED_EDGE('',*,*,#6343,.F.);
#8768=ORIENTED_EDGE('',*,*,#6338,.T.);
#8769=ORIENTED_EDGE('',*,*,#6571,.F.);
#8770=ORIENTED_EDGE('',*,*,#6342,.T.);
#8771=ORIENTED_EDGE('',*,*,#6054,.F.);
#8772=ORIENTED_EDGE('',*,*,#6344,.F.);
#8773=ORIENTED_EDGE('',*,*,#6570,.F.);
#8774=ORIENTED_EDGE('',*,*,#6335,.F.);
#8775=ORIENTED_EDGE('',*,*,#6058,.F.);
#8776=ORIENTED_EDGE('',*,*,#6572,.F.);
#8777=ORIENTED_EDGE('',*,*,#6573,.F.);
#8778=ORIENTED_EDGE('',*,*,#6574,.F.);
#8779=ORIENTED_EDGE('',*,*,#6575,.F.);
#8780=ORIENTED_EDGE('',*,*,#6337,.T.);
#8781=ORIENTED_EDGE('',*,*,#6340,.T.);
#8782=ORIENTED_EDGE('',*,*,#6341,.T.);
#8783=ORIENTED_EDGE('',*,*,#6571,.T.);
#8784=ORIENTED_EDGE('',*,*,#6400,.T.);
#8785=ORIENTED_EDGE('',*,*,#6434,.F.);
#8786=ORIENTED_EDGE('',*,*,#6348,.F.);
#8787=ORIENTED_EDGE('',*,*,#6351,.F.);
#8788=ORIENTED_EDGE('',*,*,#6576,.T.);
#8789=ORIENTED_EDGE('',*,*,#6576,.F.);
#8790=ORIENTED_EDGE('',*,*,#6350,.T.);
#8791=ORIENTED_EDGE('',*,*,#6354,.F.);
#8792=ORIENTED_EDGE('',*,*,#6435,.F.);
#8793=ORIENTED_EDGE('',*,*,#6401,.T.);
#8794=ORIENTED_EDGE('',*,*,#6404,.T.);
#8795=ORIENTED_EDGE('',*,*,#6436,.F.);
#8796=ORIENTED_EDGE('',*,*,#6358,.F.);
#8797=ORIENTED_EDGE('',*,*,#6361,.F.);
#8798=ORIENTED_EDGE('',*,*,#6577,.T.);
#8799=ORIENTED_EDGE('',*,*,#6577,.F.);
#8800=ORIENTED_EDGE('',*,*,#6360,.T.);
#8801=ORIENTED_EDGE('',*,*,#6364,.F.);
#8802=ORIENTED_EDGE('',*,*,#6381,.F.);
#8803=ORIENTED_EDGE('',*,*,#6405,.T.);
#8804=ORIENTED_EDGE('',*,*,#6554,.T.);
#8805=ORIENTED_EDGE('',*,*,#6537,.F.);
#8806=ORIENTED_EDGE('',*,*,#6555,.T.);
#8807=ORIENTED_EDGE('',*,*,#6365,.F.);
#8808=ORIENTED_EDGE('',*,*,#6369,.T.);
#8809=ORIENTED_EDGE('',*,*,#6376,.T.);
#8810=ORIENTED_EDGE('',*,*,#6578,.F.);
#8811=ORIENTED_EDGE('',*,*,#6534,.F.);
#8812=ORIENTED_EDGE('',*,*,#6553,.T.);
#8813=ORIENTED_EDGE('',*,*,#6373,.T.);
#8814=ORIENTED_EDGE('',*,*,#6552,.T.);
#8815=ORIENTED_EDGE('',*,*,#6531,.F.);
#8816=ORIENTED_EDGE('',*,*,#6578,.T.);
#8817=ORIENTED_EDGE('',*,*,#6375,.F.);
#8818=ORIENTED_EDGE('',*,*,#6379,.T.);
#8819=ORIENTED_EDGE('',*,*,#6579,.T.);
#8820=ORIENTED_EDGE('',*,*,#6383,.T.);
#8821=ORIENTED_EDGE('',*,*,#6501,.T.);
#8822=ORIENTED_EDGE('',*,*,#6505,.F.);
#8823=ORIENTED_EDGE('',*,*,#6384,.T.);
#8824=ORIENTED_EDGE('',*,*,#6579,.F.);
#8825=ORIENTED_EDGE('',*,*,#6504,.F.);
#8826=ORIENTED_EDGE('',*,*,#6580,.T.);
#8827=ORIENTED_EDGE('',*,*,#6581,.T.);
#8828=ORIENTED_EDGE('',*,*,#6581,.F.);
#8829=ORIENTED_EDGE('',*,*,#6582,.T.);
#8830=ORIENTED_EDGE('',*,*,#6583,.T.);
#8831=ORIENTED_EDGE('',*,*,#6422,.F.);
#8832=ORIENTED_EDGE('',*,*,#6385,.T.);
#8833=ORIENTED_EDGE('',*,*,#6388,.T.);
#8834=ORIENTED_EDGE('',*,*,#6412,.F.);
#8835=ORIENTED_EDGE('',*,*,#6483,.F.);
#8836=ORIENTED_EDGE('',*,*,#6485,.F.);
#8837=ORIENTED_EDGE('',*,*,#6584,.T.);
#8838=ORIENTED_EDGE('',*,*,#6584,.F.);
#8839=ORIENTED_EDGE('',*,*,#6484,.F.);
#8840=ORIENTED_EDGE('',*,*,#6486,.F.);
#8841=ORIENTED_EDGE('',*,*,#6414,.F.);
#8842=ORIENTED_EDGE('',*,*,#6389,.T.);
#8843=ORIENTED_EDGE('',*,*,#6392,.T.);
#8844=ORIENTED_EDGE('',*,*,#6460,.F.);
#8845=ORIENTED_EDGE('',*,*,#6458,.F.);
#8846=ORIENTED_EDGE('',*,*,#6481,.F.);
#8847=ORIENTED_EDGE('',*,*,#6585,.T.);
#8848=ORIENTED_EDGE('',*,*,#6585,.F.);
#8849=ORIENTED_EDGE('',*,*,#6480,.F.);
#8850=ORIENTED_EDGE('',*,*,#6482,.F.);
#8851=ORIENTED_EDGE('',*,*,#6406,.F.);
#8852=ORIENTED_EDGE('',*,*,#6393,.T.);
#8853=ORIENTED_EDGE('',*,*,#6396,.T.);
#8854=ORIENTED_EDGE('',*,*,#6431,.F.);
#8855=ORIENTED_EDGE('',*,*,#6586,.T.);
#8856=ORIENTED_EDGE('',*,*,#6587,.T.);
#8857=ORIENTED_EDGE('',*,*,#6567,.F.);
#8858=ORIENTED_EDGE('',*,*,#6588,.T.);
#8859=ORIENTED_EDGE('',*,*,#6498,.F.);
#8860=ORIENTED_EDGE('',*,*,#6419,.F.);
#8861=ORIENTED_EDGE('',*,*,#6418,.T.);
#8862=ORIENTED_EDGE('',*,*,#6488,.F.);
#8863=ORIENTED_EDGE('',*,*,#6489,.F.);
#8864=ORIENTED_EDGE('',*,*,#6425,.T.);
#8865=ORIENTED_EDGE('',*,*,#6099,.T.);
#8866=ORIENTED_EDGE('',*,*,#6423,.F.);
#8867=ORIENTED_EDGE('',*,*,#6583,.F.);
#8868=ORIENTED_EDGE('',*,*,#6566,.F.);
#8869=ORIENTED_EDGE('',*,*,#6429,.T.);
#8870=ORIENTED_EDGE('',*,*,#6565,.F.);
#8871=ORIENTED_EDGE('',*,*,#6586,.F.);
#8872=ORIENTED_EDGE('',*,*,#6432,.F.);
#8873=ORIENTED_EDGE('',*,*,#6103,.T.);
#8874=ORIENTED_EDGE('',*,*,#6439,.F.);
#8875=ORIENTED_EDGE('',*,*,#6440,.F.);
#8876=ORIENTED_EDGE('',*,*,#6589,.T.);
#8877=ORIENTED_EDGE('',*,*,#6441,.F.);
#8878=ORIENTED_EDGE('',*,*,#6443,.F.);
#8879=ORIENTED_EDGE('',*,*,#6590,.T.);
#8880=ORIENTED_EDGE('',*,*,#6445,.F.);
#8881=ORIENTED_EDGE('',*,*,#6446,.F.);
#8882=ORIENTED_EDGE('',*,*,#6591,.T.);
#8883=ORIENTED_EDGE('',*,*,#6447,.F.);
#8884=ORIENTED_EDGE('',*,*,#6449,.F.);
#8885=ORIENTED_EDGE('',*,*,#6592,.T.);
#8886=ORIENTED_EDGE('',*,*,#6451,.F.);
#8887=ORIENTED_EDGE('',*,*,#6452,.F.);
#8888=ORIENTED_EDGE('',*,*,#6593,.T.);
#8889=ORIENTED_EDGE('',*,*,#6453,.F.);
#8890=ORIENTED_EDGE('',*,*,#6455,.F.);
#8891=ORIENTED_EDGE('',*,*,#6594,.T.);
#8892=ORIENTED_EDGE('',*,*,#5872,.T.);
#8893=ORIENTED_EDGE('',*,*,#5876,.F.);
#8894=ORIENTED_EDGE('',*,*,#6467,.T.);
#8895=ORIENTED_EDGE('',*,*,#6595,.F.);
#8896=ORIENTED_EDGE('',*,*,#6523,.F.);
#8897=ORIENTED_EDGE('',*,*,#6540,.T.);
#8898=ORIENTED_EDGE('',*,*,#6464,.T.);
#8899=ORIENTED_EDGE('',*,*,#6539,.T.);
#8900=ORIENTED_EDGE('',*,*,#6520,.F.);
#8901=ORIENTED_EDGE('',*,*,#6595,.T.);
#8902=ORIENTED_EDGE('',*,*,#6466,.F.);
#8903=ORIENTED_EDGE('',*,*,#6470,.T.);
#8904=ORIENTED_EDGE('',*,*,#6477,.T.);
#8905=ORIENTED_EDGE('',*,*,#6596,.F.);
#8906=ORIENTED_EDGE('',*,*,#6525,.F.);
#8907=ORIENTED_EDGE('',*,*,#6538,.T.);
#8908=ORIENTED_EDGE('',*,*,#6474,.T.);
#8909=ORIENTED_EDGE('',*,*,#6515,.T.);
#8910=ORIENTED_EDGE('',*,*,#6526,.F.);
#8911=ORIENTED_EDGE('',*,*,#6596,.T.);
#8912=ORIENTED_EDGE('',*,*,#6476,.F.);
#8913=ORIENTED_EDGE('',*,*,#6479,.T.);
#8914=ORIENTED_EDGE('',*,*,#6499,.F.);
#8915=ORIENTED_EDGE('',*,*,#6588,.F.);
#8916=ORIENTED_EDGE('',*,*,#6490,.F.);
#8917=ORIENTED_EDGE('',*,*,#6227,.F.);
#8918=ORIENTED_EDGE('',*,*,#6493,.T.);
#8919=ORIENTED_EDGE('',*,*,#6597,.F.);
#8920=ORIENTED_EDGE('',*,*,#6497,.T.);
#8921=ORIENTED_EDGE('',*,*,#6223,.F.);
#8922=ORIENTED_EDGE('',*,*,#6598,.F.);
#8923=ORIENTED_EDGE('',*,*,#6599,.F.);
#8924=ORIENTED_EDGE('',*,*,#6600,.F.);
#8925=ORIENTED_EDGE('',*,*,#6601,.F.);
#8926=ORIENTED_EDGE('',*,*,#6492,.T.);
#8927=ORIENTED_EDGE('',*,*,#6495,.T.);
#8928=ORIENTED_EDGE('',*,*,#6496,.T.);
#8929=ORIENTED_EDGE('',*,*,#6597,.T.);
#8930=ORIENTED_EDGE('',*,*,#6516,.F.);
#8931=ORIENTED_EDGE('',*,*,#6602,.F.);
#8932=ORIENTED_EDGE('',*,*,#6509,.T.);
#8933=ORIENTED_EDGE('',*,*,#6513,.F.);
#8934=ORIENTED_EDGE('',*,*,#6602,.T.);
#8935=ORIENTED_EDGE('',*,*,#6519,.F.);
#8936=ORIENTED_EDGE('',*,*,#6603,.F.);
#8937=ORIENTED_EDGE('',*,*,#6604,.F.);
#8938=ORIENTED_EDGE('',*,*,#6510,.T.);
#8939=ORIENTED_EDGE('',*,*,#6605,.F.);
#8940=ORIENTED_EDGE('',*,*,#6603,.T.);
#8941=ORIENTED_EDGE('',*,*,#6518,.F.);
#8942=ORIENTED_EDGE('',*,*,#6542,.T.);
#8943=ORIENTED_EDGE('',*,*,#6606,.F.);
#8944=ORIENTED_EDGE('',*,*,#6550,.T.);
#8945=ORIENTED_EDGE('',*,*,#6530,.F.);
#8946=ORIENTED_EDGE('',*,*,#6558,.T.);
#8947=ORIENTED_EDGE('',*,*,#6607,.F.);
#8948=ORIENTED_EDGE('',*,*,#6608,.F.);
#8949=ORIENTED_EDGE('',*,*,#6286,.F.);
#8950=ORIENTED_EDGE('',*,*,#6545,.F.);
#8951=ORIENTED_EDGE('',*,*,#6561,.F.);
#8952=ORIENTED_EDGE('',*,*,#6606,.T.);
#8953=ORIENTED_EDGE('',*,*,#6541,.T.);
#8954=ORIENTED_EDGE('',*,*,#6562,.F.);
#8955=ORIENTED_EDGE('',*,*,#6548,.F.);
#8956=ORIENTED_EDGE('',*,*,#6282,.F.);
#8957=ORIENTED_EDGE('',*,*,#6551,.T.);
#8958=ORIENTED_EDGE('',*,*,#6608,.T.);
#8959=ORIENTED_EDGE('',*,*,#6607,.T.);
#8960=ORIENTED_EDGE('',*,*,#6557,.T.);
#8961=ORIENTED_EDGE('',*,*,#6563,.F.);
#8962=ORIENTED_EDGE('',*,*,#6582,.F.);
#8963=ORIENTED_EDGE('',*,*,#6580,.F.);
#8964=ORIENTED_EDGE('',*,*,#6559,.F.);
#8965=ORIENTED_EDGE('',*,*,#6568,.F.);
#8966=ORIENTED_EDGE('',*,*,#6587,.F.);
#8967=ORIENTED_EDGE('',*,*,#6564,.F.);
#8968=ORIENTED_EDGE('',*,*,#6604,.T.);
#8969=ORIENTED_EDGE('',*,*,#6605,.T.);
#8970=ORIENTED_EDGE('',*,*,#6560,.F.);
#8971=ORIENTED_EDGE('',*,*,#6609,.T.);
#8972=ORIENTED_EDGE('',*,*,#6610,.T.);
#8973=ORIENTED_EDGE('',*,*,#6575,.T.);
#8974=ORIENTED_EDGE('',*,*,#6611,.T.);
#8975=ORIENTED_EDGE('',*,*,#6612,.T.);
#8976=ORIENTED_EDGE('',*,*,#6613,.T.);
#8977=ORIENTED_EDGE('',*,*,#6572,.T.);
#8978=ORIENTED_EDGE('',*,*,#6610,.F.);
#8979=ORIENTED_EDGE('',*,*,#6614,.T.);
#8980=ORIENTED_EDGE('',*,*,#6615,.T.);
#8981=ORIENTED_EDGE('',*,*,#6573,.T.);
#8982=ORIENTED_EDGE('',*,*,#6613,.F.);
#8983=ORIENTED_EDGE('',*,*,#6616,.T.);
#8984=ORIENTED_EDGE('',*,*,#6611,.F.);
#8985=ORIENTED_EDGE('',*,*,#6574,.T.);
#8986=ORIENTED_EDGE('',*,*,#6615,.F.);
#8987=ORIENTED_EDGE('',*,*,#6141,.T.);
#8988=ORIENTED_EDGE('',*,*,#6139,.T.);
#8989=ORIENTED_EDGE('',*,*,#6136,.T.);
#8990=ORIENTED_EDGE('',*,*,#6589,.F.);
#8991=ORIENTED_EDGE('',*,*,#6148,.T.);
#8992=ORIENTED_EDGE('',*,*,#6145,.T.);
#8993=ORIENTED_EDGE('',*,*,#6143,.T.);
#8994=ORIENTED_EDGE('',*,*,#6590,.F.);
#8995=ORIENTED_EDGE('',*,*,#6157,.T.);
#8996=ORIENTED_EDGE('',*,*,#6155,.T.);
#8997=ORIENTED_EDGE('',*,*,#6152,.T.);
#8998=ORIENTED_EDGE('',*,*,#6591,.F.);
#8999=ORIENTED_EDGE('',*,*,#6164,.T.);
#9000=ORIENTED_EDGE('',*,*,#6161,.T.);
#9001=ORIENTED_EDGE('',*,*,#6159,.T.);
#9002=ORIENTED_EDGE('',*,*,#6592,.F.);
#9003=ORIENTED_EDGE('',*,*,#6173,.T.);
#9004=ORIENTED_EDGE('',*,*,#6171,.T.);
#9005=ORIENTED_EDGE('',*,*,#6168,.T.);
#9006=ORIENTED_EDGE('',*,*,#6593,.F.);
#9007=ORIENTED_EDGE('',*,*,#6180,.T.);
#9008=ORIENTED_EDGE('',*,*,#6177,.T.);
#9009=ORIENTED_EDGE('',*,*,#6175,.T.);
#9010=ORIENTED_EDGE('',*,*,#6594,.F.);
#9011=ORIENTED_EDGE('',*,*,#6617,.T.);
#9012=ORIENTED_EDGE('',*,*,#6618,.T.);
#9013=ORIENTED_EDGE('',*,*,#6601,.T.);
#9014=ORIENTED_EDGE('',*,*,#6619,.T.);
#9015=ORIENTED_EDGE('',*,*,#6620,.T.);
#9016=ORIENTED_EDGE('',*,*,#6621,.T.);
#9017=ORIENTED_EDGE('',*,*,#6598,.T.);
#9018=ORIENTED_EDGE('',*,*,#6618,.F.);
#9019=ORIENTED_EDGE('',*,*,#6622,.T.);
#9020=ORIENTED_EDGE('',*,*,#6623,.T.);
#9021=ORIENTED_EDGE('',*,*,#6599,.T.);
#9022=ORIENTED_EDGE('',*,*,#6621,.F.);
#9023=ORIENTED_EDGE('',*,*,#6624,.T.);
#9024=ORIENTED_EDGE('',*,*,#6619,.F.);
#9025=ORIENTED_EDGE('',*,*,#6600,.T.);
#9026=ORIENTED_EDGE('',*,*,#6623,.F.);
#9027=ORIENTED_EDGE('',*,*,#5875,.F.);
#9028=ORIENTED_EDGE('',*,*,#6614,.F.);
#9029=ORIENTED_EDGE('',*,*,#6612,.F.);
#9030=ORIENTED_EDGE('',*,*,#6609,.F.);
#9031=ORIENTED_EDGE('',*,*,#6616,.F.);
#9032=ORIENTED_EDGE('',*,*,#5881,.F.);
#9033=ORIENTED_EDGE('',*,*,#5878,.F.);
#9034=ORIENTED_EDGE('',*,*,#6622,.F.);
#9035=ORIENTED_EDGE('',*,*,#6620,.F.);
#9036=ORIENTED_EDGE('',*,*,#6617,.F.);
#9037=ORIENTED_EDGE('',*,*,#6624,.F.);
#9038=ORIENTED_EDGE('',*,*,#5884,.F.);
#9039=ORIENTED_EDGE('',*,*,#5879,.F.);
#9040=ORIENTED_EDGE('',*,*,#5882,.F.);
#9041=ORIENTED_EDGE('',*,*,#5887,.T.);
#9042=ORIENTED_EDGE('',*,*,#5885,.F.);
#9043=ORIENTED_EDGE('',*,*,#5890,.T.);
#9044=ORIENTED_EDGE('',*,*,#5888,.F.);
#9045=ORIENTED_EDGE('',*,*,#6625,.F.);
#9046=ORIENTED_EDGE('',*,*,#6626,.T.);
#9047=ORIENTED_EDGE('',*,*,#6627,.T.);
#9048=ORIENTED_EDGE('',*,*,#6626,.F.);
#9049=ORIENTED_EDGE('',*,*,#6628,.F.);
#9050=ORIENTED_EDGE('',*,*,#6629,.T.);
#9051=ORIENTED_EDGE('',*,*,#6630,.T.);
#9052=ORIENTED_EDGE('',*,*,#6629,.F.);
#9053=ORIENTED_EDGE('',*,*,#6631,.F.);
#9054=ORIENTED_EDGE('',*,*,#6632,.T.);
#9055=ORIENTED_EDGE('',*,*,#6633,.T.);
#9056=ORIENTED_EDGE('',*,*,#6632,.F.);
#9057=ORIENTED_EDGE('',*,*,#6634,.F.);
#9058=ORIENTED_EDGE('',*,*,#6635,.T.);
#9059=ORIENTED_EDGE('',*,*,#6636,.T.);
#9060=ORIENTED_EDGE('',*,*,#6635,.F.);
#9061=ORIENTED_EDGE('',*,*,#6637,.T.);
#9062=ORIENTED_EDGE('',*,*,#6638,.T.);
#9063=ORIENTED_EDGE('',*,*,#6639,.F.);
#9064=ORIENTED_EDGE('',*,*,#6638,.F.);
#9065=ORIENTED_EDGE('',*,*,#6640,.T.);
#9066=ORIENTED_EDGE('',*,*,#6641,.T.);
#9067=ORIENTED_EDGE('',*,*,#6642,.F.);
#9068=ORIENTED_EDGE('',*,*,#6641,.F.);
#9069=ORIENTED_EDGE('',*,*,#6643,.T.);
#9070=ORIENTED_EDGE('',*,*,#6644,.T.);
#9071=ORIENTED_EDGE('',*,*,#6645,.F.);
#9072=ORIENTED_EDGE('',*,*,#6644,.F.);
#9073=ORIENTED_EDGE('',*,*,#6646,.T.);
#9074=ORIENTED_EDGE('',*,*,#6647,.T.);
#9075=ORIENTED_EDGE('',*,*,#6648,.F.);
#9076=ORIENTED_EDGE('',*,*,#6647,.F.);
#9077=ORIENTED_EDGE('',*,*,#6649,.F.);
#9078=ORIENTED_EDGE('',*,*,#6650,.T.);
#9079=ORIENTED_EDGE('',*,*,#6651,.T.);
#9080=ORIENTED_EDGE('',*,*,#6650,.F.);
#9081=ORIENTED_EDGE('',*,*,#6652,.F.);
#9082=ORIENTED_EDGE('',*,*,#6653,.T.);
#9083=ORIENTED_EDGE('',*,*,#6654,.T.);
#9084=ORIENTED_EDGE('',*,*,#6653,.F.);
#9085=ORIENTED_EDGE('',*,*,#6655,.F.);
#9086=ORIENTED_EDGE('',*,*,#6656,.T.);
#9087=ORIENTED_EDGE('',*,*,#6657,.T.);
#9088=ORIENTED_EDGE('',*,*,#6656,.F.);
#9089=ORIENTED_EDGE('',*,*,#6658,.F.);
#9090=ORIENTED_EDGE('',*,*,#6659,.T.);
#9091=ORIENTED_EDGE('',*,*,#6660,.T.);
#9092=ORIENTED_EDGE('',*,*,#6659,.F.);
#9093=ORIENTED_EDGE('',*,*,#6661,.T.);
#9094=ORIENTED_EDGE('',*,*,#6662,.T.);
#9095=ORIENTED_EDGE('',*,*,#6663,.F.);
#9096=ORIENTED_EDGE('',*,*,#6662,.F.);
#9097=ORIENTED_EDGE('',*,*,#6664,.T.);
#9098=ORIENTED_EDGE('',*,*,#6665,.T.);
#9099=ORIENTED_EDGE('',*,*,#6666,.F.);
#9100=ORIENTED_EDGE('',*,*,#6665,.F.);
#9101=ORIENTED_EDGE('',*,*,#6667,.T.);
#9102=ORIENTED_EDGE('',*,*,#6668,.T.);
#9103=ORIENTED_EDGE('',*,*,#6669,.F.);
#9104=ORIENTED_EDGE('',*,*,#6668,.F.);
#9105=ORIENTED_EDGE('',*,*,#6670,.T.);
#9106=ORIENTED_EDGE('',*,*,#6671,.T.);
#9107=ORIENTED_EDGE('',*,*,#6672,.F.);
#9108=ORIENTED_EDGE('',*,*,#6671,.F.);
#9109=ORIENTED_EDGE('',*,*,#6673,.T.);
#9110=ORIENTED_EDGE('',*,*,#6674,.T.);
#9111=ORIENTED_EDGE('',*,*,#6675,.F.);
#9112=ORIENTED_EDGE('',*,*,#6674,.F.);
#9113=ORIENTED_EDGE('',*,*,#6676,.T.);
#9114=ORIENTED_EDGE('',*,*,#6677,.T.);
#9115=ORIENTED_EDGE('',*,*,#6678,.F.);
#9116=ORIENTED_EDGE('',*,*,#6677,.F.);
#9117=ORIENTED_EDGE('',*,*,#6679,.T.);
#9118=ORIENTED_EDGE('',*,*,#6680,.T.);
#9119=ORIENTED_EDGE('',*,*,#6681,.F.);
#9120=ORIENTED_EDGE('',*,*,#6680,.F.);
#9121=ORIENTED_EDGE('',*,*,#6682,.T.);
#9122=ORIENTED_EDGE('',*,*,#6683,.T.);
#9123=ORIENTED_EDGE('',*,*,#6684,.F.);
#9124=ORIENTED_EDGE('',*,*,#6683,.F.);
#9125=ORIENTED_EDGE('',*,*,#6685,.T.);
#9126=ORIENTED_EDGE('',*,*,#6686,.T.);
#9127=ORIENTED_EDGE('',*,*,#6687,.F.);
#9128=ORIENTED_EDGE('',*,*,#6686,.F.);
#9129=ORIENTED_EDGE('',*,*,#6688,.T.);
#9130=ORIENTED_EDGE('',*,*,#6689,.T.);
#9131=ORIENTED_EDGE('',*,*,#6690,.F.);
#9132=ORIENTED_EDGE('',*,*,#6689,.F.);
#9133=ORIENTED_EDGE('',*,*,#6691,.T.);
#9134=ORIENTED_EDGE('',*,*,#6692,.T.);
#9135=ORIENTED_EDGE('',*,*,#6693,.F.);
#9136=ORIENTED_EDGE('',*,*,#6692,.F.);
#9137=ORIENTED_EDGE('',*,*,#6694,.T.);
#9138=ORIENTED_EDGE('',*,*,#6695,.T.);
#9139=ORIENTED_EDGE('',*,*,#6696,.F.);
#9140=ORIENTED_EDGE('',*,*,#6695,.F.);
#9141=ORIENTED_EDGE('',*,*,#6697,.T.);
#9142=ORIENTED_EDGE('',*,*,#6698,.T.);
#9143=ORIENTED_EDGE('',*,*,#6699,.F.);
#9144=ORIENTED_EDGE('',*,*,#6698,.F.);
#9145=ORIENTED_EDGE('',*,*,#6639,.T.);
#9146=ORIENTED_EDGE('',*,*,#6700,.T.);
#9147=ORIENTED_EDGE('',*,*,#6701,.F.);
#9148=ORIENTED_EDGE('',*,*,#6700,.F.);
#9149=ORIENTED_EDGE('',*,*,#6642,.T.);
#9150=ORIENTED_EDGE('',*,*,#6702,.T.);
#9151=ORIENTED_EDGE('',*,*,#6703,.F.);
#9152=ORIENTED_EDGE('',*,*,#6702,.F.);
#9153=ORIENTED_EDGE('',*,*,#6645,.T.);
#9154=ORIENTED_EDGE('',*,*,#6704,.T.);
#9155=ORIENTED_EDGE('',*,*,#6705,.F.);
#9156=ORIENTED_EDGE('',*,*,#6704,.F.);
#9157=ORIENTED_EDGE('',*,*,#6648,.T.);
#9158=ORIENTED_EDGE('',*,*,#6706,.T.);
#9159=ORIENTED_EDGE('',*,*,#6707,.F.);
#9160=ORIENTED_EDGE('',*,*,#6706,.F.);
#9161=ORIENTED_EDGE('',*,*,#6663,.T.);
#9162=ORIENTED_EDGE('',*,*,#6708,.T.);
#9163=ORIENTED_EDGE('',*,*,#6709,.F.);
#9164=ORIENTED_EDGE('',*,*,#6708,.F.);
#9165=ORIENTED_EDGE('',*,*,#6666,.T.);
#9166=ORIENTED_EDGE('',*,*,#6710,.T.);
#9167=ORIENTED_EDGE('',*,*,#6711,.F.);
#9168=ORIENTED_EDGE('',*,*,#6710,.F.);
#9169=ORIENTED_EDGE('',*,*,#6669,.T.);
#9170=ORIENTED_EDGE('',*,*,#6712,.T.);
#9171=ORIENTED_EDGE('',*,*,#6713,.F.);
#9172=ORIENTED_EDGE('',*,*,#6712,.F.);
#9173=ORIENTED_EDGE('',*,*,#6672,.T.);
#9174=ORIENTED_EDGE('',*,*,#6714,.T.);
#9175=ORIENTED_EDGE('',*,*,#6715,.F.);
#9176=ORIENTED_EDGE('',*,*,#6714,.F.);
#9177=ORIENTED_EDGE('',*,*,#6699,.T.);
#9178=ORIENTED_EDGE('',*,*,#6716,.T.);
#9179=ORIENTED_EDGE('',*,*,#6717,.F.);
#9180=ORIENTED_EDGE('',*,*,#6716,.F.);
#9181=ORIENTED_EDGE('',*,*,#6718,.F.);
#9182=ORIENTED_EDGE('',*,*,#6719,.T.);
#9183=ORIENTED_EDGE('',*,*,#6720,.T.);
#9184=ORIENTED_EDGE('',*,*,#6719,.F.);
#9185=ORIENTED_EDGE('',*,*,#6721,.F.);
#9186=ORIENTED_EDGE('',*,*,#6722,.T.);
#9187=ORIENTED_EDGE('',*,*,#6723,.T.);
#9188=ORIENTED_EDGE('',*,*,#6722,.F.);
#9189=ORIENTED_EDGE('',*,*,#6724,.F.);
#9190=ORIENTED_EDGE('',*,*,#6725,.T.);
#9191=ORIENTED_EDGE('',*,*,#6726,.T.);
#9192=ORIENTED_EDGE('',*,*,#6725,.F.);
#9193=ORIENTED_EDGE('',*,*,#6727,.F.);
#9194=ORIENTED_EDGE('',*,*,#6728,.T.);
#9195=ORIENTED_EDGE('',*,*,#6729,.T.);
#9196=ORIENTED_EDGE('',*,*,#6728,.F.);
#9197=ORIENTED_EDGE('',*,*,#6730,.T.);
#9198=ORIENTED_EDGE('',*,*,#6731,.T.);
#9199=ORIENTED_EDGE('',*,*,#6732,.F.);
#9200=ORIENTED_EDGE('',*,*,#6731,.F.);
#9201=ORIENTED_EDGE('',*,*,#6733,.T.);
#9202=ORIENTED_EDGE('',*,*,#6734,.T.);
#9203=ORIENTED_EDGE('',*,*,#6735,.F.);
#9204=ORIENTED_EDGE('',*,*,#6734,.F.);
#9205=ORIENTED_EDGE('',*,*,#6736,.T.);
#9206=ORIENTED_EDGE('',*,*,#6737,.T.);
#9207=ORIENTED_EDGE('',*,*,#6738,.F.);
#9208=ORIENTED_EDGE('',*,*,#6737,.F.);
#9209=ORIENTED_EDGE('',*,*,#6739,.T.);
#9210=ORIENTED_EDGE('',*,*,#6740,.T.);
#9211=ORIENTED_EDGE('',*,*,#6741,.F.);
#9212=ORIENTED_EDGE('',*,*,#6740,.F.);
#9213=ORIENTED_EDGE('',*,*,#6742,.F.);
#9214=ORIENTED_EDGE('',*,*,#6743,.F.);
#9215=ORIENTED_EDGE('',*,*,#6744,.F.);
#9216=ORIENTED_EDGE('',*,*,#6745,.F.);
#9217=ORIENTED_EDGE('',*,*,#6746,.F.);
#9218=ORIENTED_EDGE('',*,*,#6747,.F.);
#9219=ORIENTED_EDGE('',*,*,#6627,.F.);
#9220=ORIENTED_EDGE('',*,*,#6630,.F.);
#9221=ORIENTED_EDGE('',*,*,#6633,.F.);
#9222=ORIENTED_EDGE('',*,*,#6636,.F.);
#9223=ORIENTED_EDGE('',*,*,#6637,.F.);
#9224=ORIENTED_EDGE('',*,*,#6640,.F.);
#9225=ORIENTED_EDGE('',*,*,#6643,.F.);
#9226=ORIENTED_EDGE('',*,*,#6646,.F.);
#9227=ORIENTED_EDGE('',*,*,#6651,.F.);
#9228=ORIENTED_EDGE('',*,*,#6654,.F.);
#9229=ORIENTED_EDGE('',*,*,#6657,.F.);
#9230=ORIENTED_EDGE('',*,*,#6660,.F.);
#9231=ORIENTED_EDGE('',*,*,#6661,.F.);
#9232=ORIENTED_EDGE('',*,*,#6664,.F.);
#9233=ORIENTED_EDGE('',*,*,#6667,.F.);
#9234=ORIENTED_EDGE('',*,*,#6670,.F.);
#9235=ORIENTED_EDGE('',*,*,#6673,.F.);
#9236=ORIENTED_EDGE('',*,*,#6676,.F.);
#9237=ORIENTED_EDGE('',*,*,#6679,.F.);
#9238=ORIENTED_EDGE('',*,*,#6682,.F.);
#9239=ORIENTED_EDGE('',*,*,#6685,.F.);
#9240=ORIENTED_EDGE('',*,*,#6688,.F.);
#9241=ORIENTED_EDGE('',*,*,#6691,.F.);
#9242=ORIENTED_EDGE('',*,*,#6694,.F.);
#9243=ORIENTED_EDGE('',*,*,#6697,.F.);
#9244=ORIENTED_EDGE('',*,*,#6748,.T.);
#9245=ORIENTED_EDGE('',*,*,#6747,.T.);
#9246=ORIENTED_EDGE('',*,*,#6749,.F.);
#9247=ORIENTED_EDGE('',*,*,#6750,.T.);
#9248=ORIENTED_EDGE('',*,*,#6751,.F.);
#9249=ORIENTED_EDGE('',*,*,#6742,.T.);
#9250=ORIENTED_EDGE('',*,*,#6748,.F.);
#9251=ORIENTED_EDGE('',*,*,#6752,.T.);
#9252=ORIENTED_EDGE('',*,*,#6753,.F.);
#9253=ORIENTED_EDGE('',*,*,#6754,.F.);
#9254=ORIENTED_EDGE('',*,*,#6755,.F.);
#9255=ORIENTED_EDGE('',*,*,#6756,.F.);
#9256=ORIENTED_EDGE('',*,*,#6757,.F.);
#9257=ORIENTED_EDGE('',*,*,#6758,.F.);
#9258=ORIENTED_EDGE('',*,*,#6759,.F.);
#9259=ORIENTED_EDGE('',*,*,#6760,.T.);
#9260=ORIENTED_EDGE('',*,*,#6761,.T.);
#9261=ORIENTED_EDGE('',*,*,#6743,.T.);
#9262=ORIENTED_EDGE('',*,*,#6761,.F.);
#9263=ORIENTED_EDGE('',*,*,#6762,.F.);
#9264=ORIENTED_EDGE('',*,*,#6763,.F.);
#9265=ORIENTED_EDGE('',*,*,#6764,.F.);
#9266=ORIENTED_EDGE('',*,*,#6744,.T.);
#9267=ORIENTED_EDGE('',*,*,#6765,.F.);
#9268=ORIENTED_EDGE('',*,*,#6766,.F.);
#9269=ORIENTED_EDGE('',*,*,#6767,.F.);
#9270=ORIENTED_EDGE('',*,*,#6768,.F.);
#9271=ORIENTED_EDGE('',*,*,#6768,.T.);
#9272=ORIENTED_EDGE('',*,*,#6769,.T.);
#9273=ORIENTED_EDGE('',*,*,#6770,.T.);
#9274=ORIENTED_EDGE('',*,*,#6745,.T.);
#9275=ORIENTED_EDGE('',*,*,#6746,.T.);
#9276=ORIENTED_EDGE('',*,*,#6770,.F.);
#9277=ORIENTED_EDGE('',*,*,#6771,.F.);
#9278=ORIENTED_EDGE('',*,*,#6772,.F.);
#9279=ORIENTED_EDGE('',*,*,#6773,.F.);
#9280=ORIENTED_EDGE('',*,*,#6774,.T.);
#9281=ORIENTED_EDGE('',*,*,#6771,.T.);
#9282=ORIENTED_EDGE('',*,*,#6769,.F.);
#9283=ORIENTED_EDGE('',*,*,#6767,.T.);
#9284=ORIENTED_EDGE('',*,*,#6775,.T.);
#9285=ORIENTED_EDGE('',*,*,#6756,.T.);
#9286=ORIENTED_EDGE('',*,*,#6625,.T.);
#9287=ORIENTED_EDGE('',*,*,#6628,.T.);
#9288=ORIENTED_EDGE('',*,*,#6631,.T.);
#9289=ORIENTED_EDGE('',*,*,#6634,.T.);
#9290=ORIENTED_EDGE('',*,*,#6701,.T.);
#9291=ORIENTED_EDGE('',*,*,#6703,.T.);
#9292=ORIENTED_EDGE('',*,*,#6705,.T.);
#9293=ORIENTED_EDGE('',*,*,#6707,.T.);
#9294=ORIENTED_EDGE('',*,*,#6649,.T.);
#9295=ORIENTED_EDGE('',*,*,#6652,.T.);
#9296=ORIENTED_EDGE('',*,*,#6655,.T.);
#9297=ORIENTED_EDGE('',*,*,#6658,.T.);
#9298=ORIENTED_EDGE('',*,*,#6709,.T.);
#9299=ORIENTED_EDGE('',*,*,#6711,.T.);
#9300=ORIENTED_EDGE('',*,*,#6713,.T.);
#9301=ORIENTED_EDGE('',*,*,#6715,.T.);
#9302=ORIENTED_EDGE('',*,*,#6717,.T.);
#9303=ORIENTED_EDGE('',*,*,#6675,.T.);
#9304=ORIENTED_EDGE('',*,*,#6678,.T.);
#9305=ORIENTED_EDGE('',*,*,#6681,.T.);
#9306=ORIENTED_EDGE('',*,*,#6684,.T.);
#9307=ORIENTED_EDGE('',*,*,#6687,.T.);
#9308=ORIENTED_EDGE('',*,*,#6690,.T.);
#9309=ORIENTED_EDGE('',*,*,#6693,.T.);
#9310=ORIENTED_EDGE('',*,*,#6696,.T.);
#9311=ORIENTED_EDGE('',*,*,#6751,.T.);
#9312=ORIENTED_EDGE('',*,*,#6776,.F.);
#9313=ORIENTED_EDGE('',*,*,#6777,.F.);
#9314=ORIENTED_EDGE('',*,*,#6778,.F.);
#9315=ORIENTED_EDGE('',*,*,#6779,.F.);
#9316=ORIENTED_EDGE('',*,*,#6780,.F.);
#9317=ORIENTED_EDGE('',*,*,#6781,.F.);
#9318=ORIENTED_EDGE('',*,*,#6752,.F.);
#9319=ORIENTED_EDGE('',*,*,#6720,.F.);
#9320=ORIENTED_EDGE('',*,*,#6723,.F.);
#9321=ORIENTED_EDGE('',*,*,#6726,.F.);
#9322=ORIENTED_EDGE('',*,*,#6729,.F.);
#9323=ORIENTED_EDGE('',*,*,#6749,.T.);
#9324=ORIENTED_EDGE('',*,*,#6773,.T.);
#9325=ORIENTED_EDGE('',*,*,#6772,.T.);
#9326=ORIENTED_EDGE('',*,*,#6782,.F.);
#9327=ORIENTED_EDGE('',*,*,#6783,.F.);
#9328=ORIENTED_EDGE('',*,*,#6764,.T.);
#9329=ORIENTED_EDGE('',*,*,#6784,.F.);
#9330=ORIENTED_EDGE('',*,*,#6785,.F.);
#9331=ORIENTED_EDGE('',*,*,#6766,.T.);
#9332=ORIENTED_EDGE('',*,*,#6765,.T.);
#9333=ORIENTED_EDGE('',*,*,#6786,.F.);
#9334=ORIENTED_EDGE('',*,*,#6787,.F.);
#9335=ORIENTED_EDGE('',*,*,#6788,.F.);
#9336=ORIENTED_EDGE('',*,*,#6789,.F.);
#9337=ORIENTED_EDGE('',*,*,#6762,.T.);
#9338=ORIENTED_EDGE('',*,*,#6760,.F.);
#9339=ORIENTED_EDGE('',*,*,#6790,.F.);
#9340=ORIENTED_EDGE('',*,*,#6791,.F.);
#9341=ORIENTED_EDGE('',*,*,#6730,.F.);
#9342=ORIENTED_EDGE('',*,*,#6733,.F.);
#9343=ORIENTED_EDGE('',*,*,#6736,.F.);
#9344=ORIENTED_EDGE('',*,*,#6739,.F.);
#9345=ORIENTED_EDGE('',*,*,#6792,.T.);
#9346=ORIENTED_EDGE('',*,*,#6793,.T.);
#9347=ORIENTED_EDGE('',*,*,#6782,.T.);
#9348=ORIENTED_EDGE('',*,*,#6774,.F.);
#9349=ORIENTED_EDGE('',*,*,#6755,.T.);
#9350=ORIENTED_EDGE('',*,*,#6785,.T.);
#9351=ORIENTED_EDGE('',*,*,#6794,.T.);
#9352=ORIENTED_EDGE('',*,*,#6795,.T.);
#9353=ORIENTED_EDGE('',*,*,#6757,.T.);
#9354=ORIENTED_EDGE('',*,*,#6775,.F.);
#9355=ORIENTED_EDGE('',*,*,#6796,.T.);
#9356=ORIENTED_EDGE('',*,*,#6797,.T.);
#9357=ORIENTED_EDGE('',*,*,#6776,.T.);
#9358=ORIENTED_EDGE('',*,*,#6798,.T.);
#9359=ORIENTED_EDGE('',*,*,#6799,.T.);
#9360=ORIENTED_EDGE('',*,*,#6797,.F.);
#9361=ORIENTED_EDGE('',*,*,#6800,.T.);
#9362=ORIENTED_EDGE('',*,*,#6801,.T.);
#9363=ORIENTED_EDGE('',*,*,#6777,.T.);
#9364=ORIENTED_EDGE('',*,*,#6802,.T.);
#9365=ORIENTED_EDGE('',*,*,#6803,.T.);
#9366=ORIENTED_EDGE('',*,*,#6804,.T.);
#9367=ORIENTED_EDGE('',*,*,#6779,.T.);
#9368=ORIENTED_EDGE('',*,*,#6805,.T.);
#9369=ORIENTED_EDGE('',*,*,#6806,.T.);
#9370=ORIENTED_EDGE('',*,*,#6780,.T.);
#9371=ORIENTED_EDGE('',*,*,#6804,.F.);
#9372=ORIENTED_EDGE('',*,*,#6806,.F.);
#9373=ORIENTED_EDGE('',*,*,#6807,.T.);
#9374=ORIENTED_EDGE('',*,*,#6753,.T.);
#9375=ORIENTED_EDGE('',*,*,#6781,.T.);
#9376=ORIENTED_EDGE('',*,*,#6750,.F.);
#9377=ORIENTED_EDGE('',*,*,#6783,.T.);
#9378=ORIENTED_EDGE('',*,*,#6793,.F.);
#9379=ORIENTED_EDGE('',*,*,#6799,.F.);
#9380=ORIENTED_EDGE('',*,*,#6798,.F.);
#9381=ORIENTED_EDGE('',*,*,#6808,.T.);
#9382=ORIENTED_EDGE('',*,*,#6809,.T.);
#9383=ORIENTED_EDGE('',*,*,#6794,.F.);
#9384=ORIENTED_EDGE('',*,*,#6784,.T.);
#9385=ORIENTED_EDGE('',*,*,#6763,.T.);
#9386=ORIENTED_EDGE('',*,*,#6810,.F.);
#9387=ORIENTED_EDGE('',*,*,#6791,.T.);
#9388=ORIENTED_EDGE('',*,*,#6811,.F.);
#9389=ORIENTED_EDGE('',*,*,#6812,.F.);
#9390=ORIENTED_EDGE('',*,*,#6810,.T.);
#9391=ORIENTED_EDGE('',*,*,#6813,.T.);
#9392=ORIENTED_EDGE('',*,*,#6814,.T.);
#9393=ORIENTED_EDGE('',*,*,#6786,.T.);
#9394=ORIENTED_EDGE('',*,*,#6815,.T.);
#9395=ORIENTED_EDGE('',*,*,#6816,.T.);
#9396=ORIENTED_EDGE('',*,*,#6817,.T.);
#9397=ORIENTED_EDGE('',*,*,#6788,.T.);
#9398=ORIENTED_EDGE('',*,*,#6789,.T.);
#9399=ORIENTED_EDGE('',*,*,#6817,.F.);
#9400=ORIENTED_EDGE('',*,*,#6818,.T.);
#9401=ORIENTED_EDGE('',*,*,#6809,.F.);
#9402=ORIENTED_EDGE('',*,*,#6808,.F.);
#9403=ORIENTED_EDGE('',*,*,#6759,.T.);
#9404=ORIENTED_EDGE('',*,*,#6819,.T.);
#9405=ORIENTED_EDGE('',*,*,#6811,.T.);
#9406=ORIENTED_EDGE('',*,*,#6790,.T.);
#9407=ORIENTED_EDGE('',*,*,#6754,.T.);
#9408=ORIENTED_EDGE('',*,*,#6807,.F.);
#9409=ORIENTED_EDGE('',*,*,#6805,.F.);
#9410=ORIENTED_EDGE('',*,*,#6803,.F.);
#9411=ORIENTED_EDGE('',*,*,#6820,.T.);
#9412=ORIENTED_EDGE('',*,*,#6800,.F.);
#9413=ORIENTED_EDGE('',*,*,#6796,.F.);
#9414=ORIENTED_EDGE('',*,*,#6792,.F.);
#9415=ORIENTED_EDGE('',*,*,#6718,.T.);
#9416=ORIENTED_EDGE('',*,*,#6721,.T.);
#9417=ORIENTED_EDGE('',*,*,#6724,.T.);
#9418=ORIENTED_EDGE('',*,*,#6727,.T.);
#9419=ORIENTED_EDGE('',*,*,#6812,.T.);
#9420=ORIENTED_EDGE('',*,*,#6819,.F.);
#9421=ORIENTED_EDGE('',*,*,#6758,.T.);
#9422=ORIENTED_EDGE('',*,*,#6795,.F.);
#9423=ORIENTED_EDGE('',*,*,#6818,.F.);
#9424=ORIENTED_EDGE('',*,*,#6816,.F.);
#9425=ORIENTED_EDGE('',*,*,#6821,.T.);
#9426=ORIENTED_EDGE('',*,*,#6813,.F.);
#9427=ORIENTED_EDGE('',*,*,#6732,.T.);
#9428=ORIENTED_EDGE('',*,*,#6735,.T.);
#9429=ORIENTED_EDGE('',*,*,#6738,.T.);
#9430=ORIENTED_EDGE('',*,*,#6741,.T.);
#9431=ORIENTED_EDGE('',*,*,#6820,.F.);
#9432=ORIENTED_EDGE('',*,*,#6802,.F.);
#9433=ORIENTED_EDGE('',*,*,#6778,.T.);
#9434=ORIENTED_EDGE('',*,*,#6801,.F.);
#9435=ORIENTED_EDGE('',*,*,#6787,.T.);
#9436=ORIENTED_EDGE('',*,*,#6814,.F.);
#9437=ORIENTED_EDGE('',*,*,#6821,.F.);
#9438=ORIENTED_EDGE('',*,*,#6815,.F.);
#9439=ORIENTED_EDGE('',*,*,#6822,.T.);
#9440=ORIENTED_EDGE('',*,*,#6823,.T.);
#9441=ORIENTED_EDGE('',*,*,#6824,.T.);
#9442=ORIENTED_EDGE('',*,*,#6823,.F.);
#9443=ORIENTED_EDGE('',*,*,#6825,.T.);
#9444=ORIENTED_EDGE('',*,*,#6826,.T.);
#9445=ORIENTED_EDGE('',*,*,#6827,.T.);
#9446=ORIENTED_EDGE('',*,*,#6826,.F.);
#9447=ORIENTED_EDGE('',*,*,#6828,.T.);
#9448=ORIENTED_EDGE('',*,*,#6829,.T.);
#9449=ORIENTED_EDGE('',*,*,#6830,.T.);
#9450=ORIENTED_EDGE('',*,*,#6829,.F.);
#9451=ORIENTED_EDGE('',*,*,#6831,.T.);
#9452=ORIENTED_EDGE('',*,*,#6832,.T.);
#9453=ORIENTED_EDGE('',*,*,#6833,.T.);
#9454=ORIENTED_EDGE('',*,*,#6832,.F.);
#9455=ORIENTED_EDGE('',*,*,#6834,.T.);
#9456=ORIENTED_EDGE('',*,*,#6835,.T.);
#9457=ORIENTED_EDGE('',*,*,#6836,.T.);
#9458=ORIENTED_EDGE('',*,*,#6835,.F.);
#9459=ORIENTED_EDGE('',*,*,#6837,.T.);
#9460=ORIENTED_EDGE('',*,*,#6838,.T.);
#9461=ORIENTED_EDGE('',*,*,#6839,.T.);
#9462=ORIENTED_EDGE('',*,*,#6838,.F.);
#9463=ORIENTED_EDGE('',*,*,#6840,.T.);
#9464=ORIENTED_EDGE('',*,*,#6841,.T.);
#9465=ORIENTED_EDGE('',*,*,#6842,.T.);
#9466=ORIENTED_EDGE('',*,*,#6841,.F.);
#9467=ORIENTED_EDGE('',*,*,#6843,.T.);
#9468=ORIENTED_EDGE('',*,*,#6844,.T.);
#9469=ORIENTED_EDGE('',*,*,#6845,.T.);
#9470=ORIENTED_EDGE('',*,*,#6844,.F.);
#9471=ORIENTED_EDGE('',*,*,#6846,.T.);
#9472=ORIENTED_EDGE('',*,*,#6847,.T.);
#9473=ORIENTED_EDGE('',*,*,#6848,.T.);
#9474=ORIENTED_EDGE('',*,*,#6847,.F.);
#9475=ORIENTED_EDGE('',*,*,#6849,.T.);
#9476=ORIENTED_EDGE('',*,*,#6850,.F.);
#9477=ORIENTED_EDGE('',*,*,#6851,.T.);
#9478=ORIENTED_EDGE('',*,*,#6852,.T.);
#9479=ORIENTED_EDGE('',*,*,#6851,.F.);
#9480=ORIENTED_EDGE('',*,*,#6853,.F.);
#9481=ORIENTED_EDGE('',*,*,#6854,.T.);
#9482=ORIENTED_EDGE('',*,*,#6855,.T.);
#9483=ORIENTED_EDGE('',*,*,#6854,.F.);
#9484=ORIENTED_EDGE('',*,*,#6856,.F.);
#9485=ORIENTED_EDGE('',*,*,#6857,.T.);
#9486=ORIENTED_EDGE('',*,*,#6858,.T.);
#9487=ORIENTED_EDGE('',*,*,#6857,.F.);
#9488=ORIENTED_EDGE('',*,*,#6859,.F.);
#9489=ORIENTED_EDGE('',*,*,#6860,.T.);
#9490=ORIENTED_EDGE('',*,*,#6861,.T.);
#9491=ORIENTED_EDGE('',*,*,#6860,.F.);
#9492=ORIENTED_EDGE('',*,*,#6862,.F.);
#9493=ORIENTED_EDGE('',*,*,#6863,.T.);
#9494=ORIENTED_EDGE('',*,*,#6864,.T.);
#9495=ORIENTED_EDGE('',*,*,#6863,.F.);
#9496=ORIENTED_EDGE('',*,*,#6865,.F.);
#9497=ORIENTED_EDGE('',*,*,#6866,.T.);
#9498=ORIENTED_EDGE('',*,*,#6867,.T.);
#9499=ORIENTED_EDGE('',*,*,#6866,.F.);
#9500=ORIENTED_EDGE('',*,*,#6868,.F.);
#9501=ORIENTED_EDGE('',*,*,#6869,.T.);
#9502=ORIENTED_EDGE('',*,*,#6870,.T.);
#9503=ORIENTED_EDGE('',*,*,#6869,.F.);
#9504=ORIENTED_EDGE('',*,*,#6871,.F.);
#9505=ORIENTED_EDGE('',*,*,#6872,.T.);
#9506=ORIENTED_EDGE('',*,*,#6873,.T.);
#9507=ORIENTED_EDGE('',*,*,#6872,.F.);
#9508=ORIENTED_EDGE('',*,*,#6874,.T.);
#9509=ORIENTED_EDGE('',*,*,#6875,.T.);
#9510=ORIENTED_EDGE('',*,*,#6876,.F.);
#9511=ORIENTED_EDGE('',*,*,#6875,.F.);
#9512=ORIENTED_EDGE('',*,*,#6846,.F.);
#9513=ORIENTED_EDGE('',*,*,#6877,.T.);
#9514=ORIENTED_EDGE('',*,*,#6878,.F.);
#9515=ORIENTED_EDGE('',*,*,#6877,.F.);
#9516=ORIENTED_EDGE('',*,*,#6849,.F.);
#9517=ORIENTED_EDGE('',*,*,#6879,.F.);
#9518=ORIENTED_EDGE('',*,*,#6880,.T.);
#9519=ORIENTED_EDGE('',*,*,#6881,.T.);
#9520=ORIENTED_EDGE('',*,*,#6882,.T.);
#9521=ORIENTED_EDGE('',*,*,#6852,.F.);
#9522=ORIENTED_EDGE('',*,*,#6855,.F.);
#9523=ORIENTED_EDGE('',*,*,#6858,.F.);
#9524=ORIENTED_EDGE('',*,*,#6861,.F.);
#9525=ORIENTED_EDGE('',*,*,#6864,.F.);
#9526=ORIENTED_EDGE('',*,*,#6867,.F.);
#9527=ORIENTED_EDGE('',*,*,#6870,.F.);
#9528=ORIENTED_EDGE('',*,*,#6873,.F.);
#9529=ORIENTED_EDGE('',*,*,#6874,.F.);
#9530=ORIENTED_EDGE('',*,*,#6848,.F.);
#9531=ORIENTED_EDGE('',*,*,#6883,.F.);
#9532=ORIENTED_EDGE('',*,*,#6884,.T.);
#9533=ORIENTED_EDGE('',*,*,#6885,.F.);
#9534=ORIENTED_EDGE('',*,*,#6886,.F.);
#9535=ORIENTED_EDGE('',*,*,#6876,.T.);
#9536=ORIENTED_EDGE('',*,*,#6850,.T.);
#9537=ORIENTED_EDGE('',*,*,#6853,.T.);
#9538=ORIENTED_EDGE('',*,*,#6856,.T.);
#9539=ORIENTED_EDGE('',*,*,#6859,.T.);
#9540=ORIENTED_EDGE('',*,*,#6862,.T.);
#9541=ORIENTED_EDGE('',*,*,#6865,.T.);
#9542=ORIENTED_EDGE('',*,*,#6868,.T.);
#9543=ORIENTED_EDGE('',*,*,#6871,.T.);
#9544=ORIENTED_EDGE('',*,*,#6878,.T.);
#9545=ORIENTED_EDGE('',*,*,#6883,.T.);
#9546=ORIENTED_EDGE('',*,*,#6887,.F.);
#9547=ORIENTED_EDGE('',*,*,#6880,.F.);
#9548=ORIENTED_EDGE('',*,*,#6888,.T.);
#9549=ORIENTED_EDGE('',*,*,#6882,.F.);
#9550=ORIENTED_EDGE('',*,*,#6889,.F.);
#9551=ORIENTED_EDGE('',*,*,#6885,.T.);
#9552=ORIENTED_EDGE('',*,*,#6890,.T.);
#9553=ORIENTED_EDGE('',*,*,#6879,.T.);
#9554=ORIENTED_EDGE('',*,*,#6890,.F.);
#9555=ORIENTED_EDGE('',*,*,#6884,.F.);
#9556=ORIENTED_EDGE('',*,*,#6888,.F.);
#9557=ORIENTED_EDGE('',*,*,#6881,.F.);
#9558=ORIENTED_EDGE('',*,*,#6887,.T.);
#9559=ORIENTED_EDGE('',*,*,#6886,.T.);
#9560=ORIENTED_EDGE('',*,*,#6889,.T.);
#9561=ORIENTED_EDGE('',*,*,#6891,.T.);
#9562=ORIENTED_EDGE('',*,*,#6892,.T.);
#9563=ORIENTED_EDGE('',*,*,#6893,.T.);
#9564=ORIENTED_EDGE('',*,*,#6892,.F.);
#9565=ORIENTED_EDGE('',*,*,#6894,.T.);
#9566=ORIENTED_EDGE('',*,*,#6895,.T.);
#9567=ORIENTED_EDGE('',*,*,#6896,.T.);
#9568=ORIENTED_EDGE('',*,*,#6895,.F.);
#9569=ORIENTED_EDGE('',*,*,#6897,.T.);
#9570=ORIENTED_EDGE('',*,*,#6898,.T.);
#9571=ORIENTED_EDGE('',*,*,#6899,.T.);
#9572=ORIENTED_EDGE('',*,*,#6898,.F.);
#9573=ORIENTED_EDGE('',*,*,#6900,.T.);
#9574=ORIENTED_EDGE('',*,*,#6901,.T.);
#9575=ORIENTED_EDGE('',*,*,#6902,.T.);
#9576=ORIENTED_EDGE('',*,*,#6903,.T.);
#9577=ORIENTED_EDGE('',*,*,#6904,.F.);
#9578=ORIENTED_EDGE('',*,*,#6905,.T.);
#9579=ORIENTED_EDGE('',*,*,#6906,.F.);
#9580=ORIENTED_EDGE('',*,*,#6905,.F.);
#9581=ORIENTED_EDGE('',*,*,#6907,.T.);
#9582=ORIENTED_EDGE('',*,*,#6908,.T.);
#9583=ORIENTED_EDGE('',*,*,#6909,.T.);
#9584=ORIENTED_EDGE('',*,*,#6908,.F.);
#9585=ORIENTED_EDGE('',*,*,#6910,.T.);
#9586=ORIENTED_EDGE('',*,*,#6911,.T.);
#9587=ORIENTED_EDGE('',*,*,#6912,.F.);
#9588=ORIENTED_EDGE('',*,*,#6913,.F.);
#9589=ORIENTED_EDGE('',*,*,#6914,.T.);
#9590=ORIENTED_EDGE('',*,*,#6915,.T.);
#9591=ORIENTED_EDGE('',*,*,#6916,.F.);
#9592=ORIENTED_EDGE('',*,*,#6917,.T.);
#9593=ORIENTED_EDGE('',*,*,#6918,.F.);
#9594=ORIENTED_EDGE('',*,*,#6919,.F.);
#9595=ORIENTED_EDGE('',*,*,#6893,.F.);
#9596=ORIENTED_EDGE('',*,*,#6896,.F.);
#9597=ORIENTED_EDGE('',*,*,#6899,.F.);
#9598=ORIENTED_EDGE('',*,*,#6920,.F.);
#9599=ORIENTED_EDGE('',*,*,#6918,.T.);
#9600=ORIENTED_EDGE('',*,*,#6921,.T.);
#9601=ORIENTED_EDGE('',*,*,#6922,.T.);
#9602=ORIENTED_EDGE('',*,*,#6914,.F.);
#9603=ORIENTED_EDGE('',*,*,#6923,.T.);
#9604=ORIENTED_EDGE('',*,*,#6924,.F.);
#9605=ORIENTED_EDGE('',*,*,#6925,.T.);
#9606=ORIENTED_EDGE('',*,*,#6926,.F.);
#9607=ORIENTED_EDGE('',*,*,#6927,.T.);
#9608=ORIENTED_EDGE('',*,*,#6928,.F.);
#9609=ORIENTED_EDGE('',*,*,#6929,.T.);
#9610=ORIENTED_EDGE('',*,*,#6916,.T.);
#9611=ORIENTED_EDGE('',*,*,#6930,.T.);
#9612=ORIENTED_EDGE('',*,*,#6931,.F.);
#9613=ORIENTED_EDGE('',*,*,#6932,.T.);
#9614=ORIENTED_EDGE('',*,*,#6924,.T.);
#9615=ORIENTED_EDGE('',*,*,#6933,.F.);
#9616=ORIENTED_EDGE('',*,*,#6934,.T.);
#9617=ORIENTED_EDGE('',*,*,#6935,.T.);
#9618=ORIENTED_EDGE('',*,*,#6936,.F.);
#9619=ORIENTED_EDGE('',*,*,#6937,.F.);
#9620=ORIENTED_EDGE('',*,*,#6922,.F.);
#9621=ORIENTED_EDGE('',*,*,#6938,.T.);
#9622=ORIENTED_EDGE('',*,*,#6931,.T.);
#9623=ORIENTED_EDGE('',*,*,#6939,.T.);
#9624=ORIENTED_EDGE('',*,*,#6891,.F.);
#9625=ORIENTED_EDGE('',*,*,#6894,.F.);
#9626=ORIENTED_EDGE('',*,*,#6897,.F.);
#9627=ORIENTED_EDGE('',*,*,#6940,.F.);
#9628=ORIENTED_EDGE('',*,*,#6941,.T.);
#9629=ORIENTED_EDGE('',*,*,#6942,.F.);
#9630=ORIENTED_EDGE('',*,*,#6943,.F.);
#9631=ORIENTED_EDGE('',*,*,#6943,.T.);
#9632=ORIENTED_EDGE('',*,*,#6944,.F.);
#9633=ORIENTED_EDGE('',*,*,#6929,.F.);
#9634=ORIENTED_EDGE('',*,*,#6945,.F.);
#9635=ORIENTED_EDGE('',*,*,#6915,.F.);
#9636=ORIENTED_EDGE('',*,*,#6925,.F.);
#9637=ORIENTED_EDGE('',*,*,#6939,.F.);
#9638=ORIENTED_EDGE('',*,*,#6930,.F.);
#9639=ORIENTED_EDGE('',*,*,#6917,.F.);
#9640=ORIENTED_EDGE('',*,*,#6932,.F.);
#9641=ORIENTED_EDGE('',*,*,#6938,.F.);
#9642=ORIENTED_EDGE('',*,*,#6921,.F.);
#9643=ORIENTED_EDGE('',*,*,#6928,.T.);
#9644=ORIENTED_EDGE('',*,*,#6946,.T.);
#9645=ORIENTED_EDGE('',*,*,#6902,.F.);
#9646=ORIENTED_EDGE('',*,*,#6947,.F.);
#9647=ORIENTED_EDGE('',*,*,#6948,.T.);
#9648=ORIENTED_EDGE('',*,*,#6910,.F.);
#9649=ORIENTED_EDGE('',*,*,#6949,.T.);
#9650=ORIENTED_EDGE('',*,*,#6936,.T.);
#9651=ORIENTED_EDGE('',*,*,#6950,.T.);
#9652=ORIENTED_EDGE('',*,*,#6940,.T.);
#9653=ORIENTED_EDGE('',*,*,#6945,.T.);
#9654=ORIENTED_EDGE('',*,*,#6906,.T.);
#9655=ORIENTED_EDGE('',*,*,#6907,.F.);
#9656=ORIENTED_EDGE('',*,*,#6951,.F.);
#9657=ORIENTED_EDGE('',*,*,#6900,.F.);
#9658=ORIENTED_EDGE('',*,*,#6952,.T.);
#9659=ORIENTED_EDGE('',*,*,#6926,.T.);
#9660=ORIENTED_EDGE('',*,*,#6944,.T.);
#9661=ORIENTED_EDGE('',*,*,#6942,.T.);
#9662=ORIENTED_EDGE('',*,*,#6953,.T.);
#9663=ORIENTED_EDGE('',*,*,#6934,.F.);
#9664=ORIENTED_EDGE('',*,*,#6954,.F.);
#9665=ORIENTED_EDGE('',*,*,#6912,.T.);
#9666=ORIENTED_EDGE('',*,*,#6955,.T.);
#9667=ORIENTED_EDGE('',*,*,#6904,.T.);
#9668=ORIENTED_EDGE('',*,*,#6909,.F.);
#9669=ORIENTED_EDGE('',*,*,#6950,.F.);
#9670=ORIENTED_EDGE('',*,*,#6935,.F.);
#9671=ORIENTED_EDGE('',*,*,#6953,.F.);
#9672=ORIENTED_EDGE('',*,*,#6941,.F.);
#9673=ORIENTED_EDGE('',*,*,#6919,.T.);
#9674=ORIENTED_EDGE('',*,*,#6920,.T.);
#9675=ORIENTED_EDGE('',*,*,#6937,.T.);
#9676=ORIENTED_EDGE('',*,*,#6949,.F.);
#9677=ORIENTED_EDGE('',*,*,#6913,.T.);
#9678=ORIENTED_EDGE('',*,*,#6954,.T.);
#9679=ORIENTED_EDGE('',*,*,#6933,.T.);
#9680=ORIENTED_EDGE('',*,*,#6923,.F.);
#9681=ORIENTED_EDGE('',*,*,#6951,.T.);
#9682=ORIENTED_EDGE('',*,*,#6956,.T.);
#9683=ORIENTED_EDGE('',*,*,#6947,.T.);
#9684=ORIENTED_EDGE('',*,*,#6901,.F.);
#9685=ORIENTED_EDGE('',*,*,#6955,.F.);
#9686=ORIENTED_EDGE('',*,*,#6911,.F.);
#9687=ORIENTED_EDGE('',*,*,#6948,.F.);
#9688=ORIENTED_EDGE('',*,*,#6956,.F.);
#9689=ORIENTED_EDGE('',*,*,#6946,.F.);
#9690=ORIENTED_EDGE('',*,*,#6927,.F.);
#9691=ORIENTED_EDGE('',*,*,#6952,.F.);
#9692=ORIENTED_EDGE('',*,*,#6903,.F.);
#9693=ORIENTED_EDGE('',*,*,#6957,.T.);
#9694=ORIENTED_EDGE('',*,*,#6958,.F.);
#9695=ORIENTED_EDGE('',*,*,#6959,.F.);
#9696=ORIENTED_EDGE('',*,*,#6960,.T.);
#9697=ORIENTED_EDGE('',*,*,#6961,.T.);
#9698=ORIENTED_EDGE('',*,*,#6962,.F.);
#9699=ORIENTED_EDGE('',*,*,#6963,.F.);
#9700=ORIENTED_EDGE('',*,*,#6958,.T.);
#9701=ORIENTED_EDGE('',*,*,#6964,.T.);
#9702=ORIENTED_EDGE('',*,*,#6965,.F.);
#9703=ORIENTED_EDGE('',*,*,#6966,.F.);
#9704=ORIENTED_EDGE('',*,*,#6962,.T.);
#9705=ORIENTED_EDGE('',*,*,#6967,.T.);
#9706=ORIENTED_EDGE('',*,*,#6960,.F.);
#9707=ORIENTED_EDGE('',*,*,#6968,.F.);
#9708=ORIENTED_EDGE('',*,*,#6965,.T.);
#9709=ORIENTED_EDGE('',*,*,#6959,.T.);
#9710=ORIENTED_EDGE('',*,*,#6963,.T.);
#9711=ORIENTED_EDGE('',*,*,#6966,.T.);
#9712=ORIENTED_EDGE('',*,*,#6968,.T.);
#9713=ORIENTED_EDGE('',*,*,#6957,.F.);
#9714=ORIENTED_EDGE('',*,*,#6967,.F.);
#9715=ORIENTED_EDGE('',*,*,#6964,.F.);
#9716=ORIENTED_EDGE('',*,*,#6961,.F.);
#9717=ORIENTED_EDGE('',*,*,#6969,.T.);
#9718=ORIENTED_EDGE('',*,*,#6970,.T.);
#9719=ORIENTED_EDGE('',*,*,#6971,.T.);
#9720=ORIENTED_EDGE('',*,*,#6970,.F.);
#9721=ORIENTED_EDGE('',*,*,#6972,.F.);
#9722=ORIENTED_EDGE('',*,*,#6973,.T.);
#9723=ORIENTED_EDGE('',*,*,#6974,.F.);
#9724=ORIENTED_EDGE('',*,*,#6973,.F.);
#9725=ORIENTED_EDGE('',*,*,#6975,.F.);
#9726=ORIENTED_EDGE('',*,*,#6976,.T.);
#9727=ORIENTED_EDGE('',*,*,#6977,.T.);
#9728=ORIENTED_EDGE('',*,*,#6976,.F.);
#9729=ORIENTED_EDGE('',*,*,#6978,.F.);
#9730=ORIENTED_EDGE('',*,*,#6979,.T.);
#9731=ORIENTED_EDGE('',*,*,#6980,.F.);
#9732=ORIENTED_EDGE('',*,*,#6979,.F.);
#9733=ORIENTED_EDGE('',*,*,#6981,.F.);
#9734=ORIENTED_EDGE('',*,*,#6982,.T.);
#9735=ORIENTED_EDGE('',*,*,#6983,.T.);
#9736=ORIENTED_EDGE('',*,*,#6982,.F.);
#9737=ORIENTED_EDGE('',*,*,#6984,.F.);
#9738=ORIENTED_EDGE('',*,*,#6985,.T.);
#9739=ORIENTED_EDGE('',*,*,#6986,.T.);
#9740=ORIENTED_EDGE('',*,*,#6987,.T.);
#9741=ORIENTED_EDGE('',*,*,#6988,.F.);
#9742=ORIENTED_EDGE('',*,*,#6989,.T.);
#9743=ORIENTED_EDGE('',*,*,#6984,.T.);
#9744=ORIENTED_EDGE('',*,*,#6990,.T.);
#9745=ORIENTED_EDGE('',*,*,#6991,.T.);
#9746=ORIENTED_EDGE('',*,*,#6992,.F.);
#9747=ORIENTED_EDGE('',*,*,#6975,.T.);
#9748=ORIENTED_EDGE('',*,*,#6981,.T.);
#9749=ORIENTED_EDGE('',*,*,#6993,.T.);
#9750=ORIENTED_EDGE('',*,*,#6994,.F.);
#9751=ORIENTED_EDGE('',*,*,#6995,.F.);
#9752=ORIENTED_EDGE('',*,*,#6992,.T.);
#9753=ORIENTED_EDGE('',*,*,#6996,.F.);
#9754=ORIENTED_EDGE('',*,*,#6997,.T.);
#9755=ORIENTED_EDGE('',*,*,#6998,.F.);
#9756=ORIENTED_EDGE('',*,*,#6994,.T.);
#9757=ORIENTED_EDGE('',*,*,#6999,.T.);
#9758=ORIENTED_EDGE('',*,*,#7000,.T.);
#9759=ORIENTED_EDGE('',*,*,#6974,.T.);
#9760=ORIENTED_EDGE('',*,*,#6980,.T.);
#9761=ORIENTED_EDGE('',*,*,#7001,.F.);
#9762=ORIENTED_EDGE('',*,*,#7002,.T.);
#9763=ORIENTED_EDGE('',*,*,#6996,.T.);
#9764=ORIENTED_EDGE('',*,*,#7003,.T.);
#9765=ORIENTED_EDGE('',*,*,#7004,.T.);
#9766=ORIENTED_EDGE('',*,*,#7005,.T.);
#9767=ORIENTED_EDGE('',*,*,#7006,.F.);
#9768=ORIENTED_EDGE('',*,*,#7007,.T.);
#9769=ORIENTED_EDGE('',*,*,#7001,.T.);
#9770=ORIENTED_EDGE('',*,*,#7008,.T.);
#9771=ORIENTED_EDGE('',*,*,#6972,.T.);
#9772=ORIENTED_EDGE('',*,*,#6978,.T.);
#9773=ORIENTED_EDGE('',*,*,#7009,.F.);
#9774=ORIENTED_EDGE('',*,*,#7010,.T.);
#9775=ORIENTED_EDGE('',*,*,#7011,.T.);
#9776=ORIENTED_EDGE('',*,*,#7012,.T.);
#9777=ORIENTED_EDGE('',*,*,#6986,.F.);
#9778=ORIENTED_EDGE('',*,*,#7013,.T.);
#9779=ORIENTED_EDGE('',*,*,#6977,.F.);
#9780=ORIENTED_EDGE('',*,*,#6983,.F.);
#9781=ORIENTED_EDGE('',*,*,#7006,.T.);
#9782=ORIENTED_EDGE('',*,*,#7014,.T.);
#9783=ORIENTED_EDGE('',*,*,#7015,.T.);
#9784=ORIENTED_EDGE('',*,*,#7016,.T.);
#9785=ORIENTED_EDGE('',*,*,#7017,.F.);
#9786=ORIENTED_EDGE('',*,*,#7018,.T.);
#9787=ORIENTED_EDGE('',*,*,#7009,.T.);
#9788=ORIENTED_EDGE('',*,*,#7019,.T.);
#9789=ORIENTED_EDGE('',*,*,#6988,.T.);
#9790=ORIENTED_EDGE('',*,*,#6995,.T.);
#9791=ORIENTED_EDGE('',*,*,#6998,.T.);
#9792=ORIENTED_EDGE('',*,*,#7020,.T.);
#9793=ORIENTED_EDGE('',*,*,#7021,.F.);
#9794=ORIENTED_EDGE('',*,*,#7022,.T.);
#9795=ORIENTED_EDGE('',*,*,#7004,.F.);
#9796=ORIENTED_EDGE('',*,*,#7023,.T.);
#9797=ORIENTED_EDGE('',*,*,#6999,.F.);
#9798=ORIENTED_EDGE('',*,*,#6993,.F.);
#9799=ORIENTED_EDGE('',*,*,#6991,.F.);
#9800=ORIENTED_EDGE('',*,*,#7024,.T.);
#9801=ORIENTED_EDGE('',*,*,#7011,.F.);
#9802=ORIENTED_EDGE('',*,*,#7025,.T.);
#9803=ORIENTED_EDGE('',*,*,#7026,.T.);
#9804=ORIENTED_EDGE('',*,*,#7027,.F.);
#9805=ORIENTED_EDGE('',*,*,#6997,.F.);
#9806=ORIENTED_EDGE('',*,*,#7002,.F.);
#9807=ORIENTED_EDGE('',*,*,#7007,.F.);
#9808=ORIENTED_EDGE('',*,*,#7020,.F.);
#9809=ORIENTED_EDGE('',*,*,#7000,.F.);
#9810=ORIENTED_EDGE('',*,*,#7023,.F.);
#9811=ORIENTED_EDGE('',*,*,#7008,.F.);
#9812=ORIENTED_EDGE('',*,*,#7003,.F.);
#9813=ORIENTED_EDGE('',*,*,#7013,.F.);
#9814=ORIENTED_EDGE('',*,*,#6985,.F.);
#9815=ORIENTED_EDGE('',*,*,#6989,.F.);
#9816=ORIENTED_EDGE('',*,*,#7019,.F.);
#9817=ORIENTED_EDGE('',*,*,#7012,.F.);
#9818=ORIENTED_EDGE('',*,*,#7024,.F.);
#9819=ORIENTED_EDGE('',*,*,#6990,.F.);
#9820=ORIENTED_EDGE('',*,*,#6987,.F.);
#9821=ORIENTED_EDGE('',*,*,#7028,.F.);
#9822=ORIENTED_EDGE('',*,*,#7029,.T.);
#9823=ORIENTED_EDGE('',*,*,#7030,.F.);
#9824=ORIENTED_EDGE('',*,*,#7031,.F.);
#9825=ORIENTED_EDGE('',*,*,#7032,.F.);
#9826=ORIENTED_EDGE('',*,*,#7031,.T.);
#9827=ORIENTED_EDGE('',*,*,#7033,.F.);
#9828=ORIENTED_EDGE('',*,*,#7034,.T.);
#9829=ORIENTED_EDGE('',*,*,#7035,.F.);
#9830=ORIENTED_EDGE('',*,*,#7036,.T.);
#9831=ORIENTED_EDGE('',*,*,#7037,.F.);
#9832=ORIENTED_EDGE('',*,*,#7029,.F.);
#9833=ORIENTED_EDGE('',*,*,#7036,.F.);
#9834=ORIENTED_EDGE('',*,*,#7038,.T.);
#9835=ORIENTED_EDGE('',*,*,#7027,.T.);
#9836=ORIENTED_EDGE('',*,*,#7039,.T.);
#9837=ORIENTED_EDGE('',*,*,#7016,.F.);
#9838=ORIENTED_EDGE('',*,*,#7040,.T.);
#9839=ORIENTED_EDGE('',*,*,#7034,.F.);
#9840=ORIENTED_EDGE('',*,*,#7041,.T.);
#9841=ORIENTED_EDGE('',*,*,#7042,.T.);
#9842=ORIENTED_EDGE('',*,*,#7041,.F.);
#9843=ORIENTED_EDGE('',*,*,#7033,.T.);
#9844=ORIENTED_EDGE('',*,*,#7030,.T.);
#9845=ORIENTED_EDGE('',*,*,#7037,.T.);
#9846=ORIENTED_EDGE('',*,*,#7039,.F.);
#9847=ORIENTED_EDGE('',*,*,#6971,.F.);
#9848=ORIENTED_EDGE('',*,*,#7026,.F.);
#9849=ORIENTED_EDGE('',*,*,#7043,.T.);
#9850=ORIENTED_EDGE('',*,*,#7017,.T.);
#9851=ORIENTED_EDGE('',*,*,#7042,.F.);
#9852=ORIENTED_EDGE('',*,*,#7035,.T.);
#9853=ORIENTED_EDGE('',*,*,#7028,.T.);
#9854=ORIENTED_EDGE('',*,*,#7032,.T.);
#9855=ORIENTED_EDGE('',*,*,#7040,.F.);
#9856=ORIENTED_EDGE('',*,*,#7044,.F.);
#9857=ORIENTED_EDGE('',*,*,#7038,.F.);
#9858=ORIENTED_EDGE('',*,*,#6969,.F.);
#9859=ORIENTED_EDGE('',*,*,#7015,.F.);
#9860=ORIENTED_EDGE('',*,*,#7045,.T.);
#9861=ORIENTED_EDGE('',*,*,#7021,.T.);
#9862=ORIENTED_EDGE('',*,*,#7044,.T.);
#9863=ORIENTED_EDGE('',*,*,#7022,.F.);
#9864=ORIENTED_EDGE('',*,*,#7045,.F.);
#9865=ORIENTED_EDGE('',*,*,#7014,.F.);
#9866=ORIENTED_EDGE('',*,*,#7005,.F.);
#9867=ORIENTED_EDGE('',*,*,#7025,.F.);
#9868=ORIENTED_EDGE('',*,*,#7010,.F.);
#9869=ORIENTED_EDGE('',*,*,#7018,.F.);
#9870=ORIENTED_EDGE('',*,*,#7043,.F.);
#9871=ORIENTED_EDGE('',*,*,#7046,.F.);
#9872=ORIENTED_EDGE('',*,*,#7047,.T.);
#9873=ORIENTED_EDGE('',*,*,#7048,.T.);
#9874=ORIENTED_EDGE('',*,*,#7047,.F.);
#9875=ORIENTED_EDGE('',*,*,#7049,.F.);
#9876=ORIENTED_EDGE('',*,*,#7050,.T.);
#9877=ORIENTED_EDGE('',*,*,#7051,.T.);
#9878=ORIENTED_EDGE('',*,*,#7050,.F.);
#9879=ORIENTED_EDGE('',*,*,#7052,.F.);
#9880=ORIENTED_EDGE('',*,*,#7053,.F.);
#9881=ORIENTED_EDGE('',*,*,#7054,.T.);
#9882=ORIENTED_EDGE('',*,*,#7049,.T.);
#9883=ORIENTED_EDGE('',*,*,#7054,.F.);
#9884=ORIENTED_EDGE('',*,*,#7052,.T.);
#9885=ORIENTED_EDGE('',*,*,#7053,.T.);
#9886=ORIENTED_EDGE('',*,*,#7055,.T.);
#9887=ORIENTED_EDGE('',*,*,#7056,.F.);
#9888=ORIENTED_EDGE('',*,*,#7055,.F.);
#9889=ORIENTED_EDGE('',*,*,#7048,.F.);
#9890=ORIENTED_EDGE('',*,*,#7057,.T.);
#9891=ORIENTED_EDGE('',*,*,#7058,.T.);
#9892=ORIENTED_EDGE('',*,*,#7057,.F.);
#9893=ORIENTED_EDGE('',*,*,#7059,.F.);
#9894=ORIENTED_EDGE('',*,*,#7060,.T.);
#9895=ORIENTED_EDGE('',*,*,#7046,.T.);
#9896=ORIENTED_EDGE('',*,*,#7060,.F.);
#9897=ORIENTED_EDGE('',*,*,#7059,.T.);
#9898=ORIENTED_EDGE('',*,*,#7051,.F.);
#9899=ORIENTED_EDGE('',*,*,#7058,.F.);
#9900=ORIENTED_EDGE('',*,*,#7056,.T.);
#9901=ORIENTED_EDGE('',*,*,#7061,.T.);
#9902=ORIENTED_EDGE('',*,*,#7061,.F.);
#9903=ORIENTED_EDGE('',*,*,#7062,.T.);
#9904=ORIENTED_EDGE('',*,*,#7062,.F.);
#9905=ORIENTED_EDGE('',*,*,#7063,.T.);
#9906=ORIENTED_EDGE('',*,*,#7063,.F.);
#9907=ORIENTED_EDGE('',*,*,#7064,.T.);
#9908=ORIENTED_EDGE('',*,*,#7064,.F.);
#9909=ORIENTED_EDGE('',*,*,#7065,.T.);
#9910=ORIENTED_EDGE('',*,*,#7065,.F.);
#9911=ORIENTED_EDGE('',*,*,#7066,.T.);
#9912=ORIENTED_EDGE('',*,*,#7066,.F.);
#9913=ORIENTED_EDGE('',*,*,#7067,.T.);
#9914=ORIENTED_EDGE('',*,*,#7067,.F.);
#9915=ORIENTED_EDGE('',*,*,#7068,.T.);
#9916=ORIENTED_EDGE('',*,*,#7068,.F.);
#9917=ORIENTED_EDGE('',*,*,#7069,.T.);
#9918=ORIENTED_EDGE('',*,*,#7069,.F.);
#9919=ORIENTED_EDGE('',*,*,#7070,.T.);
#9920=ORIENTED_EDGE('',*,*,#7070,.F.);
#9921=ORIENTED_EDGE('',*,*,#7071,.T.);
#9922=ORIENTED_EDGE('',*,*,#7071,.F.);
#9923=ORIENTED_EDGE('',*,*,#7072,.T.);
#9924=ORIENTED_EDGE('',*,*,#7072,.F.);
#9925=ORIENTED_EDGE('',*,*,#7073,.F.);
#9926=ORIENTED_EDGE('',*,*,#7074,.T.);
#9927=ORIENTED_EDGE('',*,*,#7075,.T.);
#9928=ORIENTED_EDGE('',*,*,#7074,.F.);
#9929=ORIENTED_EDGE('',*,*,#7076,.F.);
#9930=ORIENTED_EDGE('',*,*,#7077,.T.);
#9931=ORIENTED_EDGE('',*,*,#7078,.T.);
#9932=ORIENTED_EDGE('',*,*,#7077,.F.);
#9933=ORIENTED_EDGE('',*,*,#7073,.T.);
#9934=ORIENTED_EDGE('',*,*,#7078,.F.);
#9935=ORIENTED_EDGE('',*,*,#7075,.F.);
#9936=ORIENTED_EDGE('',*,*,#7076,.T.);
#9937=ORIENTED_EDGE('',*,*,#7079,.F.);
#9938=ORIENTED_EDGE('',*,*,#7080,.T.);
#9939=ORIENTED_EDGE('',*,*,#7081,.T.);
#9940=ORIENTED_EDGE('',*,*,#7080,.F.);
#9941=ORIENTED_EDGE('',*,*,#7082,.F.);
#9942=ORIENTED_EDGE('',*,*,#7083,.T.);
#9943=ORIENTED_EDGE('',*,*,#7084,.T.);
#9944=ORIENTED_EDGE('',*,*,#7083,.F.);
#9945=ORIENTED_EDGE('',*,*,#7081,.F.);
#9946=ORIENTED_EDGE('',*,*,#7082,.T.);
#9947=ORIENTED_EDGE('',*,*,#7079,.T.);
#9948=ORIENTED_EDGE('',*,*,#7084,.F.);
#9949=ORIENTED_EDGE('',*,*,#7085,.F.);
#9950=ORIENTED_EDGE('',*,*,#7086,.T.);
#9951=ORIENTED_EDGE('',*,*,#7087,.T.);
#9952=ORIENTED_EDGE('',*,*,#7086,.F.);
#9953=ORIENTED_EDGE('',*,*,#7088,.F.);
#9954=ORIENTED_EDGE('',*,*,#7089,.T.);
#9955=ORIENTED_EDGE('',*,*,#7090,.T.);
#9956=ORIENTED_EDGE('',*,*,#7089,.F.);
#9957=ORIENTED_EDGE('',*,*,#7091,.F.);
#9958=ORIENTED_EDGE('',*,*,#7092,.T.);
#9959=ORIENTED_EDGE('',*,*,#7088,.T.);
#9960=ORIENTED_EDGE('',*,*,#7092,.F.);
#9961=ORIENTED_EDGE('',*,*,#7093,.F.);
#9962=ORIENTED_EDGE('',*,*,#7094,.T.);
#9963=ORIENTED_EDGE('',*,*,#7091,.T.);
#9964=ORIENTED_EDGE('',*,*,#7094,.F.);
#9965=ORIENTED_EDGE('',*,*,#7095,.F.);
#9966=ORIENTED_EDGE('',*,*,#7096,.F.);
#9967=ORIENTED_EDGE('',*,*,#7097,.T.);
#9968=ORIENTED_EDGE('',*,*,#7098,.T.);
#9969=ORIENTED_EDGE('',*,*,#7097,.F.);
#9970=ORIENTED_EDGE('',*,*,#7095,.T.);
#9971=ORIENTED_EDGE('',*,*,#7096,.T.);
#9972=ORIENTED_EDGE('',*,*,#7099,.T.);
#9973=ORIENTED_EDGE('',*,*,#7100,.F.);
#9974=ORIENTED_EDGE('',*,*,#7099,.F.);
#9975=ORIENTED_EDGE('',*,*,#7085,.T.);
#9976=ORIENTED_EDGE('',*,*,#7093,.T.);
#9977=ORIENTED_EDGE('',*,*,#7100,.T.);
#9978=ORIENTED_EDGE('',*,*,#7090,.F.);
#9979=ORIENTED_EDGE('',*,*,#7087,.F.);
#9980=ORIENTED_EDGE('',*,*,#7098,.F.);
#9981=ORIENTED_EDGE('',*,*,#7101,.F.);
#9982=ORIENTED_EDGE('',*,*,#7102,.T.);
#9983=ORIENTED_EDGE('',*,*,#7103,.T.);
#9984=ORIENTED_EDGE('',*,*,#7102,.F.);
#9985=ORIENTED_EDGE('',*,*,#7104,.T.);
#9986=ORIENTED_EDGE('',*,*,#7105,.T.);
#9987=ORIENTED_EDGE('',*,*,#7106,.F.);
#9988=ORIENTED_EDGE('',*,*,#7105,.F.);
#9989=ORIENTED_EDGE('',*,*,#7107,.F.);
#9990=ORIENTED_EDGE('',*,*,#7108,.T.);
#9991=ORIENTED_EDGE('',*,*,#7109,.F.);
#9992=ORIENTED_EDGE('',*,*,#7108,.F.);
#9993=ORIENTED_EDGE('',*,*,#7109,.T.);
#9994=ORIENTED_EDGE('',*,*,#7104,.F.);
#9995=ORIENTED_EDGE('',*,*,#7101,.T.);
#9996=ORIENTED_EDGE('',*,*,#7106,.T.);
#9997=ORIENTED_EDGE('',*,*,#7103,.F.);
#9998=ORIENTED_EDGE('',*,*,#7107,.T.);
#9999=ORIENTED_EDGE('',*,*,#7110,.F.);
#10000=ORIENTED_EDGE('',*,*,#7111,.T.);
#10001=ORIENTED_EDGE('',*,*,#7112,.T.);
#10002=ORIENTED_EDGE('',*,*,#7111,.F.);
#10003=ORIENTED_EDGE('',*,*,#7113,.T.);
#10004=ORIENTED_EDGE('',*,*,#7114,.T.);
#10005=ORIENTED_EDGE('',*,*,#7115,.F.);
#10006=ORIENTED_EDGE('',*,*,#7114,.F.);
#10007=ORIENTED_EDGE('',*,*,#7116,.F.);
#10008=ORIENTED_EDGE('',*,*,#7117,.T.);
#10009=ORIENTED_EDGE('',*,*,#7118,.F.);
#10010=ORIENTED_EDGE('',*,*,#7117,.F.);
#10011=ORIENTED_EDGE('',*,*,#7118,.T.);
#10012=ORIENTED_EDGE('',*,*,#7113,.F.);
#10013=ORIENTED_EDGE('',*,*,#7110,.T.);
#10014=ORIENTED_EDGE('',*,*,#7115,.T.);
#10015=ORIENTED_EDGE('',*,*,#7112,.F.);
#10016=ORIENTED_EDGE('',*,*,#7116,.T.);
#10017=ORIENTED_EDGE('',*,*,#7119,.F.);
#10018=ORIENTED_EDGE('',*,*,#7120,.T.);
#10019=ORIENTED_EDGE('',*,*,#7121,.T.);
#10020=ORIENTED_EDGE('',*,*,#7120,.F.);
#10021=ORIENTED_EDGE('',*,*,#7122,.F.);
#10022=ORIENTED_EDGE('',*,*,#7123,.T.);
#10023=ORIENTED_EDGE('',*,*,#7119,.T.);
#10024=ORIENTED_EDGE('',*,*,#7123,.F.);
#10025=ORIENTED_EDGE('',*,*,#7124,.F.);
#10026=ORIENTED_EDGE('',*,*,#7125,.T.);
#10027=ORIENTED_EDGE('',*,*,#7126,.T.);
#10028=ORIENTED_EDGE('',*,*,#7125,.F.);
#10029=ORIENTED_EDGE('',*,*,#7127,.F.);
#10030=ORIENTED_EDGE('',*,*,#7128,.T.);
#10031=ORIENTED_EDGE('',*,*,#7124,.T.);
#10032=ORIENTED_EDGE('',*,*,#7128,.F.);
#10033=ORIENTED_EDGE('',*,*,#7129,.F.);
#10034=ORIENTED_EDGE('',*,*,#7130,.T.);
#10035=ORIENTED_EDGE('',*,*,#7131,.T.);
#10036=ORIENTED_EDGE('',*,*,#7132,.F.);
#10037=ORIENTED_EDGE('',*,*,#7133,.T.);
#10038=ORIENTED_EDGE('',*,*,#7134,.T.);
#10039=ORIENTED_EDGE('',*,*,#7129,.T.);
#10040=ORIENTED_EDGE('',*,*,#7135,.T.);
#10041=ORIENTED_EDGE('',*,*,#7121,.F.);
#10042=ORIENTED_EDGE('',*,*,#7126,.F.);
#10043=ORIENTED_EDGE('',*,*,#7136,.F.);
#10044=ORIENTED_EDGE('',*,*,#7137,.F.);
#10045=ORIENTED_EDGE('',*,*,#7131,.F.);
#10046=ORIENTED_EDGE('',*,*,#7138,.F.);
#10047=ORIENTED_EDGE('',*,*,#7122,.T.);
#10048=ORIENTED_EDGE('',*,*,#7127,.T.);
#10049=ORIENTED_EDGE('',*,*,#7136,.T.);
#10050=ORIENTED_EDGE('',*,*,#7139,.F.);
#10051=ORIENTED_EDGE('',*,*,#7133,.F.);
#10052=ORIENTED_EDGE('',*,*,#7140,.T.);
#10053=ORIENTED_EDGE('',*,*,#7138,.T.);
#10054=ORIENTED_EDGE('',*,*,#7130,.F.);
#10055=ORIENTED_EDGE('',*,*,#7134,.F.);
#10056=ORIENTED_EDGE('',*,*,#7139,.T.);
#10057=ORIENTED_EDGE('',*,*,#7137,.T.);
#10058=ORIENTED_EDGE('',*,*,#7140,.F.);
#10059=ORIENTED_EDGE('',*,*,#7135,.F.);
#10060=ORIENTED_EDGE('',*,*,#7132,.T.);
#10061=ORIENTED_EDGE('',*,*,#7141,.T.);
#10062=ORIENTED_EDGE('',*,*,#7142,.T.);
#10063=ORIENTED_EDGE('',*,*,#7143,.T.);
#10064=ORIENTED_EDGE('',*,*,#7144,.T.);
#10065=ORIENTED_EDGE('',*,*,#7145,.T.);
#10066=ORIENTED_EDGE('',*,*,#7146,.T.);
#10067=ORIENTED_EDGE('',*,*,#7147,.T.);
#10068=ORIENTED_EDGE('',*,*,#7141,.F.);
#10069=ORIENTED_EDGE('',*,*,#7148,.F.);
#10070=ORIENTED_EDGE('',*,*,#7149,.T.);
#10071=ORIENTED_EDGE('',*,*,#7150,.F.);
#10072=ORIENTED_EDGE('',*,*,#7149,.F.);
#10073=ORIENTED_EDGE('',*,*,#7151,.F.);
#10074=ORIENTED_EDGE('',*,*,#7152,.T.);
#10075=ORIENTED_EDGE('',*,*,#7153,.T.);
#10076=ORIENTED_EDGE('',*,*,#7152,.F.);
#10077=ORIENTED_EDGE('',*,*,#7153,.F.);
#10078=ORIENTED_EDGE('',*,*,#7154,.T.);
#10079=ORIENTED_EDGE('',*,*,#7148,.T.);
#10080=ORIENTED_EDGE('',*,*,#7154,.F.);
#10081=ORIENTED_EDGE('',*,*,#7150,.T.);
#10082=ORIENTED_EDGE('',*,*,#7155,.T.);
#10083=ORIENTED_EDGE('',*,*,#7156,.T.);
#10084=ORIENTED_EDGE('',*,*,#7155,.F.);
#10085=ORIENTED_EDGE('',*,*,#7156,.F.);
#10086=ORIENTED_EDGE('',*,*,#7157,.T.);
#10087=ORIENTED_EDGE('',*,*,#7158,.T.);
#10088=ORIENTED_EDGE('',*,*,#7157,.F.);
#10089=ORIENTED_EDGE('',*,*,#7151,.T.);
#10090=ORIENTED_EDGE('',*,*,#7159,.T.);
#10091=ORIENTED_EDGE('',*,*,#7160,.T.);
#10092=ORIENTED_EDGE('',*,*,#7161,.T.);
#10093=ORIENTED_EDGE('',*,*,#7162,.T.);
#10094=ORIENTED_EDGE('',*,*,#7163,.T.);
#10095=ORIENTED_EDGE('',*,*,#7164,.T.);
#10096=ORIENTED_EDGE('',*,*,#7158,.F.);
#10097=ORIENTED_EDGE('',*,*,#7160,.F.);
#10098=ORIENTED_EDGE('',*,*,#7165,.F.);
#10099=ORIENTED_EDGE('',*,*,#7166,.T.);
#10100=ORIENTED_EDGE('',*,*,#7167,.T.);
#10101=ORIENTED_EDGE('',*,*,#7168,.T.);
#10102=ORIENTED_EDGE('',*,*,#7161,.F.);
#10103=ORIENTED_EDGE('',*,*,#7168,.F.);
#10104=ORIENTED_EDGE('',*,*,#7169,.T.);
#10105=ORIENTED_EDGE('',*,*,#7170,.T.);
#10106=ORIENTED_EDGE('',*,*,#7171,.T.);
#10107=ORIENTED_EDGE('',*,*,#7162,.F.);
#10108=ORIENTED_EDGE('',*,*,#7171,.F.);
#10109=ORIENTED_EDGE('',*,*,#7172,.T.);
#10110=ORIENTED_EDGE('',*,*,#7173,.T.);
#10111=ORIENTED_EDGE('',*,*,#7174,.T.);
#10112=ORIENTED_EDGE('',*,*,#7163,.F.);
#10113=ORIENTED_EDGE('',*,*,#7174,.F.);
#10114=ORIENTED_EDGE('',*,*,#7175,.T.);
#10115=ORIENTED_EDGE('',*,*,#7176,.T.);
#10116=ORIENTED_EDGE('',*,*,#7177,.T.);
#10117=ORIENTED_EDGE('',*,*,#7164,.F.);
#10118=ORIENTED_EDGE('',*,*,#7177,.F.);
#10119=ORIENTED_EDGE('',*,*,#7178,.T.);
#10120=ORIENTED_EDGE('',*,*,#7179,.T.);
#10121=ORIENTED_EDGE('',*,*,#7180,.T.);
#10122=ORIENTED_EDGE('',*,*,#7159,.F.);
#10123=ORIENTED_EDGE('',*,*,#7180,.F.);
#10124=ORIENTED_EDGE('',*,*,#7181,.T.);
#10125=ORIENTED_EDGE('',*,*,#7182,.T.);
#10126=ORIENTED_EDGE('',*,*,#7165,.T.);
#10127=ORIENTED_EDGE('',*,*,#7144,.F.);
#10128=ORIENTED_EDGE('',*,*,#7181,.F.);
#10129=ORIENTED_EDGE('',*,*,#7179,.F.);
#10130=ORIENTED_EDGE('',*,*,#7143,.F.);
#10131=ORIENTED_EDGE('',*,*,#7166,.F.);
#10132=ORIENTED_EDGE('',*,*,#7182,.F.);
#10133=ORIENTED_EDGE('',*,*,#7142,.F.);
#10134=ORIENTED_EDGE('',*,*,#7169,.F.);
#10135=ORIENTED_EDGE('',*,*,#7167,.F.);
#10136=ORIENTED_EDGE('',*,*,#7147,.F.);
#10137=ORIENTED_EDGE('',*,*,#7172,.F.);
#10138=ORIENTED_EDGE('',*,*,#7170,.F.);
#10139=ORIENTED_EDGE('',*,*,#7146,.F.);
#10140=ORIENTED_EDGE('',*,*,#7175,.F.);
#10141=ORIENTED_EDGE('',*,*,#7173,.F.);
#10142=ORIENTED_EDGE('',*,*,#7145,.F.);
#10143=ORIENTED_EDGE('',*,*,#7178,.F.);
#10144=ORIENTED_EDGE('',*,*,#7176,.F.);
#10145=CYLINDRICAL_SURFACE('',#11106,1.25);
#10146=CYLINDRICAL_SURFACE('',#11109,1.25);
#10147=CYLINDRICAL_SURFACE('',#11112,1.25);
#10148=CYLINDRICAL_SURFACE('',#11115,1.25);
#10149=CYLINDRICAL_SURFACE('',#11118,1.25);
#10150=CYLINDRICAL_SURFACE('',#11121,1.25);
#10151=CYLINDRICAL_SURFACE('',#11124,1.25);
#10152=CYLINDRICAL_SURFACE('',#11127,1.25);
#10153=CYLINDRICAL_SURFACE('',#11130,1.25);
#10154=CYLINDRICAL_SURFACE('',#11133,1.25);
#10155=CYLINDRICAL_SURFACE('',#11136,1.25);
#10156=CYLINDRICAL_SURFACE('',#11139,1.25);
#10157=CYLINDRICAL_SURFACE('',#11142,1.25);
#10158=CYLINDRICAL_SURFACE('',#11145,1.25);
#10159=CYLINDRICAL_SURFACE('',#11148,1.25);
#10160=CYLINDRICAL_SURFACE('',#11151,1.25);
#10161=CYLINDRICAL_SURFACE('',#11154,5.);
#10162=CYLINDRICAL_SURFACE('',#11184,3.);
#10163=CYLINDRICAL_SURFACE('',#11186,3.);
#10164=CYLINDRICAL_SURFACE('',#11198,6.);
#10165=CYLINDRICAL_SURFACE('',#11200,6.);
#10166=CYLINDRICAL_SURFACE('',#11207,2.5);
#10167=CYLINDRICAL_SURFACE('',#11208,2.5);
#10168=CYLINDRICAL_SURFACE('',#11209,2.5);
#10169=CYLINDRICAL_SURFACE('',#11210,2.5);
#10170=CYLINDRICAL_SURFACE('',#11211,2.5);
#10171=CYLINDRICAL_SURFACE('',#11212,2.5);
#10172=CYLINDRICAL_SURFACE('',#11213,2.5);
#10173=CYLINDRICAL_SURFACE('',#11214,2.5);
#10174=CYLINDRICAL_SURFACE('',#11216,5.5);
#10175=CYLINDRICAL_SURFACE('',#11219,14.);
#10176=CYLINDRICAL_SURFACE('',#11222,1.35);
#10177=CYLINDRICAL_SURFACE('',#11225,1.35);
#10178=CYLINDRICAL_SURFACE('',#11228,1.35);
#10179=CYLINDRICAL_SURFACE('',#11231,1.35);
#10180=CYLINDRICAL_SURFACE('',#11234,1.35);
#10181=CYLINDRICAL_SURFACE('',#11237,1.35);
#10182=CYLINDRICAL_SURFACE('',#11240,1.35);
#10183=CYLINDRICAL_SURFACE('',#11243,1.35);
#10184=CYLINDRICAL_SURFACE('',#11246,1.35);
#10185=CYLINDRICAL_SURFACE('',#11249,1.35);
#10186=CYLINDRICAL_SURFACE('',#11252,1.35);
#10187=CYLINDRICAL_SURFACE('',#11255,1.35);
#10188=CYLINDRICAL_SURFACE('',#11258,5.);
#10189=CYLINDRICAL_SURFACE('',#11261,7.5);
#10190=CYLINDRICAL_SURFACE('',#11264,2.75);
#10191=CYLINDRICAL_SURFACE('',#11267,5.);
#10192=CYLINDRICAL_SURFACE('',#11270,7.25);
#10193=CYLINDRICAL_SURFACE('',#11273,14.);
#10194=CYLINDRICAL_SURFACE('',#11276,4.75);
#10195=CYLINDRICAL_SURFACE('',#11279,2.75);
#10196=CYLINDRICAL_SURFACE('',#11283,2.);
#10197=CYLINDRICAL_SURFACE('',#11286,1.5);
#10198=CYLINDRICAL_SURFACE('',#11289,1.5);
#10199=CYLINDRICAL_SURFACE('',#11292,1.5);
#10200=CYLINDRICAL_SURFACE('',#11306,2.);
#10201=CYLINDRICAL_SURFACE('',#11309,2.);
#10202=CYLINDRICAL_SURFACE('',#11312,2.);
#10203=CYLINDRICAL_SURFACE('',#11335,3.5);
#10204=CYLINDRICAL_SURFACE('',#11338,2.);
#10205=CYLINDRICAL_SURFACE('',#11340,2.);
#10206=CYLINDRICAL_SURFACE('',#11343,2.);
#10207=CYLINDRICAL_SURFACE('',#11346,1.5);
#10208=CYLINDRICAL_SURFACE('',#11348,1.5);
#10209=CYLINDRICAL_SURFACE('',#11359,0.999999999999999);
#10210=CYLINDRICAL_SURFACE('',#11361,0.999999999999999);
#10211=CYLINDRICAL_SURFACE('',#11369,3.);
#10212=CYLINDRICAL_SURFACE('',#11372,3.);
#10213=CYLINDRICAL_SURFACE('',#11375,3.);
#10214=CYLINDRICAL_SURFACE('',#11380,3.);
#10215=CYLINDRICAL_SURFACE('',#11385,3.);
#10216=CYLINDRICAL_SURFACE('',#11388,3.);
#10217=CYLINDRICAL_SURFACE('',#11394,2.35);
#10218=CYLINDRICAL_SURFACE('',#11397,0.999999999999999);
#10219=CYLINDRICAL_SURFACE('',#11400,0.999999999999999);
#10220=CYLINDRICAL_SURFACE('',#11403,2.35);
#10221=CYLINDRICAL_SURFACE('',#11406,1.);
#10222=CYLINDRICAL_SURFACE('',#11409,1.);
#10223=CYLINDRICAL_SURFACE('',#11412,2.35);
#10224=CYLINDRICAL_SURFACE('',#11415,0.999999999999999);
#10225=CYLINDRICAL_SURFACE('',#11418,0.999999999999999);
#10226=CYLINDRICAL_SURFACE('',#11421,2.35);
#10227=CYLINDRICAL_SURFACE('',#11438,3.);
#10228=CYLINDRICAL_SURFACE('',#11441,3.);
#10229=CYLINDRICAL_SURFACE('',#11446,3.);
#10230=CYLINDRICAL_SURFACE('',#11451,3.);
#10231=CYLINDRICAL_SURFACE('',#11454,3.);
#10232=CYLINDRICAL_SURFACE('',#11456,3.);
#10233=CYLINDRICAL_SURFACE('',#11464,2.);
#10234=CYLINDRICAL_SURFACE('',#11521,1.5);
#10235=CYLINDRICAL_SURFACE('',#11525,1.5);
#10236=CYLINDRICAL_SURFACE('',#11527,1.5);
#10237=CYLINDRICAL_SURFACE('',#11530,1.5);
#10238=CYLINDRICAL_SURFACE('',#11535,1.5);
#10239=CYLINDRICAL_SURFACE('',#11537,1.5);
#10240=CYLINDRICAL_SURFACE('',#11540,1.5);
#10241=CYLINDRICAL_SURFACE('',#11545,1.5);
#10242=CYLINDRICAL_SURFACE('',#11547,1.5);
#10243=CYLINDRICAL_SURFACE('',#11550,1.5);
#10244=CYLINDRICAL_SURFACE('',#11555,1.5);
#10245=CYLINDRICAL_SURFACE('',#11584,2.);
#10246=CYLINDRICAL_SURFACE('',#11675,1.25);
#10247=CYLINDRICAL_SURFACE('',#11678,1.25);
#10248=CYLINDRICAL_SURFACE('',#11681,1.25);
#10249=CYLINDRICAL_SURFACE('',#11684,1.25);
#10250=CYLINDRICAL_SURFACE('',#11687,1.025);
#10251=CYLINDRICAL_SURFACE('',#11690,1.025);
#10252=CYLINDRICAL_SURFACE('',#11693,1.025);
#10253=CYLINDRICAL_SURFACE('',#11696,1.025);
#10254=CYLINDRICAL_SURFACE('',#11699,1.25);
#10255=CYLINDRICAL_SURFACE('',#11702,1.25);
#10256=CYLINDRICAL_SURFACE('',#11705,1.25);
#10257=CYLINDRICAL_SURFACE('',#11708,1.25);
#10258=CYLINDRICAL_SURFACE('',#11711,1.025);
#10259=CYLINDRICAL_SURFACE('',#11714,1.025);
#10260=CYLINDRICAL_SURFACE('',#11717,1.025);
#10261=CYLINDRICAL_SURFACE('',#11720,1.025);
#10262=CYLINDRICAL_SURFACE('',#11723,1.25);
#10263=CYLINDRICAL_SURFACE('',#11726,1.25);
#10264=CYLINDRICAL_SURFACE('',#11729,1.25);
#10265=CYLINDRICAL_SURFACE('',#11732,1.25);
#10266=CYLINDRICAL_SURFACE('',#11735,1.25);
#10267=CYLINDRICAL_SURFACE('',#11738,1.25);
#10268=CYLINDRICAL_SURFACE('',#11741,1.25);
#10269=CYLINDRICAL_SURFACE('',#11744,1.25);
#10270=CYLINDRICAL_SURFACE('',#11747,5.);
#10271=CYLINDRICAL_SURFACE('',#11768,1.3);
#10272=CYLINDRICAL_SURFACE('',#11771,1.3);
#10273=CYLINDRICAL_SURFACE('',#11774,1.3);
#10274=CYLINDRICAL_SURFACE('',#11777,1.3);
#10275=CYLINDRICAL_SURFACE('',#11780,1.3);
#10276=CYLINDRICAL_SURFACE('',#11783,1.3);
#10277=CYLINDRICAL_SURFACE('',#11786,1.3);
#10278=CYLINDRICAL_SURFACE('',#11789,1.3);
#10279=CYLINDRICAL_SURFACE('',#11795,0.5);
#10280=CYLINDRICAL_SURFACE('',#11802,0.5);
#10281=CYLINDRICAL_SURFACE('',#11804,6.);
#10282=CYLINDRICAL_SURFACE('',#11807,6.);
#10283=CYLINDRICAL_SURFACE('',#11818,2.5);
#10284=CYLINDRICAL_SURFACE('',#11820,2.5);
#10285=CYLINDRICAL_SURFACE('',#11823,2.);
#10286=CYLINDRICAL_SURFACE('',#11825,2.);
#10287=CYLINDRICAL_SURFACE('',#11828,2.);
#10288=CYLINDRICAL_SURFACE('',#11831,2.);
#10289=CYLINDRICAL_SURFACE('',#11833,2.);
#10290=CYLINDRICAL_SURFACE('',#11836,2.);
#10291=CYLINDRICAL_SURFACE('',#11842,1.25);
#10292=CYLINDRICAL_SURFACE('',#11845,1.25);
#10293=CYLINDRICAL_SURFACE('',#11848,1.25);
#10294=CYLINDRICAL_SURFACE('',#11851,1.25);
#10295=CYLINDRICAL_SURFACE('',#11854,1.25);
#10296=CYLINDRICAL_SURFACE('',#11857,1.25);
#10297=CYLINDRICAL_SURFACE('',#11860,1.25);
#10298=CYLINDRICAL_SURFACE('',#11863,1.25);
#10299=CYLINDRICAL_SURFACE('',#11871,1.25);
#10300=CYLINDRICAL_SURFACE('',#11874,1.25);
#10301=CYLINDRICAL_SURFACE('',#11877,1.25);
#10302=CYLINDRICAL_SURFACE('',#11880,1.25);
#10303=CYLINDRICAL_SURFACE('',#11883,1.25);
#10304=CYLINDRICAL_SURFACE('',#11886,1.25);
#10305=CYLINDRICAL_SURFACE('',#11889,1.25);
#10306=CYLINDRICAL_SURFACE('',#11892,1.25);
#10307=CYLINDRICAL_SURFACE('',#11895,5.5);
#10308=CYLINDRICAL_SURFACE('',#11898,2.5);
#10309=CYLINDRICAL_SURFACE('',#11906,14.);
#10310=CYLINDRICAL_SURFACE('',#11907,9.);
#10311=CYLINDRICAL_SURFACE('',#11912,12.5);
#10312=CYLINDRICAL_SURFACE('',#11915,12.5);
#10313=CYLINDRICAL_SURFACE('',#11918,12.5);
#10314=CYLINDRICAL_SURFACE('',#11921,12.);
#10315=CYLINDRICAL_SURFACE('',#11924,8.);
#10316=CYLINDRICAL_SURFACE('',#11927,8.);
#10317=CYLINDRICAL_SURFACE('',#11937,12.);
#10318=CYLINDRICAL_SURFACE('',#11950,10.);
#10319=CYLINDRICAL_SURFACE('',#11954,10.);
#10320=CYLINDRICAL_SURFACE('',#11955,10.);
#10321=CYLINDRICAL_SURFACE('',#11965,8.);
#10322=CYLINDRICAL_SURFACE('',#11968,1.25);
#10323=CYLINDRICAL_SURFACE('',#11971,1.25);
#10324=CYLINDRICAL_SURFACE('',#11974,1.25);
#10325=CYLINDRICAL_SURFACE('',#11977,1.25);
#10326=CYLINDRICAL_SURFACE('',#11993,12.);
#10327=CYLINDRICAL_SURFACE('',#11998,10.);
#10328=CYLINDRICAL_SURFACE('',#12001,10.);
#10329=CYLINDRICAL_SURFACE('',#12018,4.);
#10330=CYLINDRICAL_SURFACE('',#12023,5.51648351648352);
#10331=CYLINDRICAL_SURFACE('',#12025,5.51648351648352);
#10332=CYLINDRICAL_SURFACE('',#12053,6.48351648351648);
#10333=CYLINDRICAL_SURFACE('',#12056,5.51648351648352);
#10334=CYLINDRICAL_SURFACE('',#12061,6.48351648351649);
#10335=CYLINDRICAL_SURFACE('',#12064,5.51648351648352);
#10336=CYLINDRICAL_SURFACE('',#12069,9.);
#10337=CYLINDRICAL_SURFACE('',#12072,6.48351648351648);
#10338=CYLINDRICAL_SURFACE('',#12078,6.48351648351648);
#10339=CYLINDRICAL_SURFACE('',#12080,8.);
#10340=CYLINDRICAL_SURFACE('',#12090,5.);
#10341=CYLINDRICAL_SURFACE('',#12093,2.1);
#10342=CYLINDRICAL_SURFACE('',#12096,4.);
#10343=CYLINDRICAL_SURFACE('',#12103,5.);
#10344=CYLINDRICAL_SURFACE('',#12106,1.6);
#10345=CYLINDRICAL_SURFACE('',#12109,4.);
#10346=CYLINDRICAL_SURFACE('',#12134,2.24999999999999);
#10347=CYLINDRICAL_SURFACE('',#12139,2.24999999999999);
#10348=CYLINDRICAL_SURFACE('',#12141,10.);
#10349=CYLINDRICAL_SURFACE('',#12148,10.);
#10350=CYLINDRICAL_SURFACE('',#12163,3.9);
#10351=CYLINDRICAL_SURFACE('',#12167,2.);
#10352=ADVANCED_FACE('',(#900),#10145,.F.);
#10353=ADVANCED_FACE('',(#901),#10146,.F.);
#10354=ADVANCED_FACE('',(#902),#10147,.F.);
#10355=ADVANCED_FACE('',(#903),#10148,.F.);
#10356=ADVANCED_FACE('',(#904),#10149,.F.);
#10357=ADVANCED_FACE('',(#905),#10150,.F.);
#10358=ADVANCED_FACE('',(#906),#10151,.F.);
#10359=ADVANCED_FACE('',(#907),#10152,.F.);
#10360=ADVANCED_FACE('',(#908),#10153,.F.);
#10361=ADVANCED_FACE('',(#909),#10154,.F.);
#10362=ADVANCED_FACE('',(#910),#10155,.F.);
#10363=ADVANCED_FACE('',(#911),#10156,.F.);
#10364=ADVANCED_FACE('',(#912),#10157,.F.);
#10365=ADVANCED_FACE('',(#913),#10158,.F.);
#10366=ADVANCED_FACE('',(#914),#10159,.F.);
#10367=ADVANCED_FACE('',(#915),#10160,.F.);
#10368=ADVANCED_FACE('',(#916),#10161,.F.);
#10369=ADVANCED_FACE('',(#917),#576,.T.);
#10370=ADVANCED_FACE('',(#918),#577,.T.);
#10371=ADVANCED_FACE('',(#919),#578,.T.);
#10372=ADVANCED_FACE('',(#920),#579,.T.);
#10373=ADVANCED_FACE('',(#921),#580,.T.);
#10374=ADVANCED_FACE('',(#922),#581,.T.);
#10375=ADVANCED_FACE('',(#923),#582,.T.);
#10376=ADVANCED_FACE('',(#924),#583,.T.);
#10377=ADVANCED_FACE('',(#925,#380,#381,#382,#383),#584,.F.);
#10378=ADVANCED_FACE('',(#926),#585,.T.);
#10379=ADVANCED_FACE('',(#927,#384,#385,#386,#387),#586,.T.);
#10380=ADVANCED_FACE('',(#928),#10162,.F.);
#10381=ADVANCED_FACE('',(#929,#388,#389,#390,#391,#392,#393,#394,#395,#396),
#587,.T.);
#10382=ADVANCED_FACE('',(#930),#10163,.F.);
#10383=ADVANCED_FACE('',(#931,#397,#398,#399,#400),#588,.T.);
#10384=ADVANCED_FACE('',(#932),#589,.T.);
#10385=ADVANCED_FACE('',(#933,#401,#402,#403,#404),#590,.F.);
#10386=ADVANCED_FACE('',(#934),#10164,.T.);
#10387=ADVANCED_FACE('',(#935,#405,#406,#407,#408,#409,#410,#411,#412,#413),
#591,.F.);
#10388=ADVANCED_FACE('',(#936),#10165,.T.);
#10389=ADVANCED_FACE('',(#937),#592,.F.);
#10390=ADVANCED_FACE('',(#938),#593,.T.);
#10391=ADVANCED_FACE('',(#939),#594,.F.);
#10392=ADVANCED_FACE('',(#940),#595,.F.);
#10393=ADVANCED_FACE('',(#941),#596,.F.);
#10394=ADVANCED_FACE('',(#942),#597,.T.);
#10395=ADVANCED_FACE('',(#943),#10166,.T.);
#10396=ADVANCED_FACE('',(#944),#10167,.T.);
#10397=ADVANCED_FACE('',(#945),#10168,.T.);
#10398=ADVANCED_FACE('',(#946),#10169,.T.);
#10399=ADVANCED_FACE('',(#947),#10170,.T.);
#10400=ADVANCED_FACE('',(#948),#10171,.T.);
#10401=ADVANCED_FACE('',(#949),#10172,.T.);
#10402=ADVANCED_FACE('',(#950),#10173,.T.);
#10403=ADVANCED_FACE('',(#951),#10174,.T.);
#10404=ADVANCED_FACE('',(#952),#10175,.T.);
#10405=ADVANCED_FACE('',(#953),#10176,.F.);
#10406=ADVANCED_FACE('',(#954),#10177,.F.);
#10407=ADVANCED_FACE('',(#955),#10178,.F.);
#10408=ADVANCED_FACE('',(#956),#10179,.F.);
#10409=ADVANCED_FACE('',(#957),#10180,.F.);
#10410=ADVANCED_FACE('',(#958),#10181,.F.);
#10411=ADVANCED_FACE('',(#959),#10182,.F.);
#10412=ADVANCED_FACE('',(#960),#10183,.F.);
#10413=ADVANCED_FACE('',(#961),#10184,.F.);
#10414=ADVANCED_FACE('',(#962),#10185,.F.);
#10415=ADVANCED_FACE('',(#963),#10186,.F.);
#10416=ADVANCED_FACE('',(#964),#10187,.F.);
#10417=ADVANCED_FACE('',(#965),#10188,.T.);
#10418=ADVANCED_FACE('',(#966),#10189,.F.);
#10419=ADVANCED_FACE('',(#967),#10190,.T.);
#10420=ADVANCED_FACE('',(#968),#10191,.T.);
#10421=ADVANCED_FACE('',(#969),#10192,.T.);
#10422=ADVANCED_FACE('',(#970),#10193,.T.);
#10423=ADVANCED_FACE('',(#971),#10194,.T.);
#10424=ADVANCED_FACE('',(#972),#10195,.T.);
#10425=ADVANCED_FACE('',(#973,#414),#598,.T.);
#10426=ADVANCED_FACE('',(#974),#10196,.T.);
#10427=ADVANCED_FACE('',(#975),#10197,.T.);
#10428=ADVANCED_FACE('',(#976),#10198,.T.);
#10429=ADVANCED_FACE('',(#977),#10199,.T.);
#10430=ADVANCED_FACE('',(#978,#415),#599,.F.);
#10431=ADVANCED_FACE('',(#979),#600,.T.);
#10432=ADVANCED_FACE('',(#980),#292,.F.);
#10433=ADVANCED_FACE('',(#981),#293,.F.);
#10434=ADVANCED_FACE('',(#982),#601,.T.);
#10435=ADVANCED_FACE('',(#983),#244,.T.);
#10436=ADVANCED_FACE('',(#984),#602,.T.);
#10437=ADVANCED_FACE('',(#985),#245,.T.);
#10438=ADVANCED_FACE('',(#986),#603,.T.);
#10439=ADVANCED_FACE('',(#987),#10200,.T.);
#10440=ADVANCED_FACE('',(#988),#10201,.T.);
#10441=ADVANCED_FACE('',(#989),#10202,.T.);
#10442=ADVANCED_FACE('',(#990,#416,#417,#418,#419,#420,#421),#604,.F.);
#10443=ADVANCED_FACE('',(#991),#10203,.T.);
#10444=ADVANCED_FACE('',(#992),#10204,.T.);
#10445=ADVANCED_FACE('',(#993),#10205,.T.);
#10446=ADVANCED_FACE('',(#994),#10206,.T.);
#10447=ADVANCED_FACE('',(#995),#10207,.T.);
#10448=ADVANCED_FACE('',(#996),#10208,.T.);
#10449=ADVANCED_FACE('',(#997,#422,#423,#424,#425,#426,#427),#605,.T.);
#10450=ADVANCED_FACE('',(#998),#10209,.T.);
#10451=ADVANCED_FACE('',(#999),#232,.T.);
#10452=ADVANCED_FACE('',(#1000),#10210,.T.);
#10453=ADVANCED_FACE('',(#1001),#233,.T.);
#10454=ADVANCED_FACE('',(#1002,#428),#606,.F.);
#10455=ADVANCED_FACE('',(#1003),#607,.T.);
#10456=ADVANCED_FACE('',(#1004),#608,.F.);
#10457=ADVANCED_FACE('',(#1005),#609,.T.);
#10458=ADVANCED_FACE('',(#1006),#610,.T.);
#10459=ADVANCED_FACE('',(#1007),#611,.F.);
#10460=ADVANCED_FACE('',(#1008),#10211,.T.);
#10461=ADVANCED_FACE('',(#1009),#612,.F.);
#10462=ADVANCED_FACE('',(#1010),#10212,.T.);
#10463=ADVANCED_FACE('',(#1011),#613,.F.);
#10464=ADVANCED_FACE('',(#1012),#10213,.T.);
#10465=ADVANCED_FACE('',(#1013),#614,.F.);
#10466=ADVANCED_FACE('',(#1014),#10214,.T.);
#10467=ADVANCED_FACE('',(#1015),#615,.F.);
#10468=ADVANCED_FACE('',(#1016),#10215,.T.);
#10469=ADVANCED_FACE('',(#1017),#616,.F.);
#10470=ADVANCED_FACE('',(#1018),#10216,.T.);
#10471=ADVANCED_FACE('',(#1019),#223,.T.);
#10472=ADVANCED_FACE('',(#1020),#617,.F.);
#10473=ADVANCED_FACE('',(#1021),#10217,.F.);
#10474=ADVANCED_FACE('',(#1022),#618,.F.);
#10475=ADVANCED_FACE('',(#1023),#10218,.T.);
#10476=ADVANCED_FACE('',(#1024),#619,.T.);
#10477=ADVANCED_FACE('',(#1025),#10219,.T.);
#10478=ADVANCED_FACE('',(#1026),#620,.F.);
#10479=ADVANCED_FACE('',(#1027),#10220,.F.);
#10480=ADVANCED_FACE('',(#1028),#621,.F.);
#10481=ADVANCED_FACE('',(#1029),#10221,.T.);
#10482=ADVANCED_FACE('',(#1030),#622,.T.);
#10483=ADVANCED_FACE('',(#1031),#10222,.T.);
#10484=ADVANCED_FACE('',(#1032),#623,.F.);
#10485=ADVANCED_FACE('',(#1033),#10223,.F.);
#10486=ADVANCED_FACE('',(#1034),#624,.F.);
#10487=ADVANCED_FACE('',(#1035),#10224,.T.);
#10488=ADVANCED_FACE('',(#1036),#625,.T.);
#10489=ADVANCED_FACE('',(#1037),#10225,.T.);
#10490=ADVANCED_FACE('',(#1038),#626,.F.);
#10491=ADVANCED_FACE('',(#1039),#10226,.F.);
#10492=ADVANCED_FACE('',(#1040),#627,.F.);
#10493=ADVANCED_FACE('',(#1041),#224,.T.);
#10494=ADVANCED_FACE('',(#1042),#628,.F.);
#10495=ADVANCED_FACE('',(#1043,#429),#629,.F.);
#10496=ADVANCED_FACE('',(#1044),#630,.T.);
#10497=ADVANCED_FACE('',(#1045),#631,.F.);
#10498=ADVANCED_FACE('',(#1046),#632,.T.);
#10499=ADVANCED_FACE('',(#1047),#633,.T.);
#10500=ADVANCED_FACE('',(#1048),#634,.T.);
#10501=ADVANCED_FACE('',(#1049),#10227,.T.);
#10502=ADVANCED_FACE('',(#1050),#635,.T.);
#10503=ADVANCED_FACE('',(#1051),#10228,.T.);
#10504=ADVANCED_FACE('',(#1052),#636,.T.);
#10505=ADVANCED_FACE('',(#1053),#10229,.T.);
#10506=ADVANCED_FACE('',(#1054),#637,.T.);
#10507=ADVANCED_FACE('',(#1055),#10230,.T.);
#10508=ADVANCED_FACE('',(#1056),#638,.T.);
#10509=ADVANCED_FACE('',(#1057),#10231,.T.);
#10510=ADVANCED_FACE('',(#1058),#10232,.T.);
#10511=ADVANCED_FACE('',(#1059),#639,.F.);
#10512=ADVANCED_FACE('',(#1060),#640,.F.);
#10513=ADVANCED_FACE('',(#1061),#641,.T.);
#10514=ADVANCED_FACE('',(#1062),#642,.T.);
#10515=ADVANCED_FACE('',(#1063),#643,.F.);
#10516=ADVANCED_FACE('',(#1064),#10233,.T.);
#10517=ADVANCED_FACE('',(#1065),#644,.T.);
#10518=ADVANCED_FACE('',(#1066),#645,.F.);
#10519=ADVANCED_FACE('',(#1067),#646,.F.);
#10520=ADVANCED_FACE('',(#1068),#647,.T.);
#10521=ADVANCED_FACE('',(#1069),#648,.T.);
#10522=ADVANCED_FACE('',(#1070),#649,.F.);
#10523=ADVANCED_FACE('',(#1071),#650,.F.);
#10524=ADVANCED_FACE('',(#1072),#651,.F.);
#10525=ADVANCED_FACE('',(#1073),#652,.T.);
#10526=ADVANCED_FACE('',(#1074),#653,.T.);
#10527=ADVANCED_FACE('',(#1075),#654,.T.);
#10528=ADVANCED_FACE('',(#1076),#655,.T.);
#10529=ADVANCED_FACE('',(#1077),#656,.F.);
#10530=ADVANCED_FACE('',(#1078),#657,.T.);
#10531=ADVANCED_FACE('',(#1079),#658,.F.);
#10532=ADVANCED_FACE('',(#1080),#659,.T.);
#10533=ADVANCED_FACE('',(#1081),#660,.T.);
#10534=ADVANCED_FACE('',(#1082),#661,.T.);
#10535=ADVANCED_FACE('',(#1083),#662,.F.);
#10536=ADVANCED_FACE('',(#1084),#663,.F.);
#10537=ADVANCED_FACE('',(#1085),#664,.F.);
#10538=ADVANCED_FACE('',(#1086),#665,.T.);
#10539=ADVANCED_FACE('',(#1087),#666,.F.);
#10540=ADVANCED_FACE('',(#1088),#667,.T.);
#10541=ADVANCED_FACE('',(#1089),#668,.F.);
#10542=ADVANCED_FACE('',(#1090),#669,.F.);
#10543=ADVANCED_FACE('',(#1091),#670,.F.);
#10544=ADVANCED_FACE('',(#1092),#671,.T.);
#10545=ADVANCED_FACE('',(#1093),#672,.F.);
#10546=ADVANCED_FACE('',(#1094),#673,.T.);
#10547=ADVANCED_FACE('',(#1095),#674,.T.);
#10548=ADVANCED_FACE('',(#1096,#430),#675,.F.);
#10549=ADVANCED_FACE('',(#1097,#431),#676,.F.);
#10550=ADVANCED_FACE('',(#1098,#432),#677,.F.);
#10551=ADVANCED_FACE('',(#1099,#433),#678,.F.);
#10552=ADVANCED_FACE('',(#1100,#434),#679,.F.);
#10553=ADVANCED_FACE('',(#1101,#435),#680,.F.);
#10554=ADVANCED_FACE('',(#1102),#681,.T.);
#10555=ADVANCED_FACE('',(#1103),#682,.F.);
#10556=ADVANCED_FACE('',(#1104),#683,.T.);
#10557=ADVANCED_FACE('',(#1105),#684,.F.);
#10558=ADVANCED_FACE('',(#1106),#685,.T.);
#10559=ADVANCED_FACE('',(#1107),#686,.T.);
#10560=ADVANCED_FACE('',(#1108),#687,.F.);
#10561=ADVANCED_FACE('',(#1109),#688,.T.);
#10562=ADVANCED_FACE('',(#1110),#689,.F.);
#10563=ADVANCED_FACE('',(#1111),#690,.T.);
#10564=ADVANCED_FACE('',(#1112),#691,.F.);
#10565=ADVANCED_FACE('',(#1113),#692,.T.);
#10566=ADVANCED_FACE('',(#1114),#693,.F.);
#10567=ADVANCED_FACE('',(#1115),#694,.T.);
#10568=ADVANCED_FACE('',(#1116),#695,.F.);
#10569=ADVANCED_FACE('',(#1117),#696,.T.);
#10570=ADVANCED_FACE('',(#1118),#697,.T.);
#10571=ADVANCED_FACE('',(#1119),#698,.T.);
#10572=ADVANCED_FACE('',(#1120),#10234,.T.);
#10573=ADVANCED_FACE('',(#1121),#225,.T.);
#10574=ADVANCED_FACE('',(#1122),#10235,.T.);
#10575=ADVANCED_FACE('',(#1123),#10236,.T.);
#10576=ADVANCED_FACE('',(#1124),#10237,.T.);
#10577=ADVANCED_FACE('',(#1125),#226,.T.);
#10578=ADVANCED_FACE('',(#1126),#10238,.T.);
#10579=ADVANCED_FACE('',(#1127),#10239,.T.);
#10580=ADVANCED_FACE('',(#1128),#10240,.T.);
#10581=ADVANCED_FACE('',(#1129),#227,.T.);
#10582=ADVANCED_FACE('',(#1130),#10241,.T.);
#10583=ADVANCED_FACE('',(#1131),#10242,.T.);
#10584=ADVANCED_FACE('',(#1132),#10243,.T.);
#10585=ADVANCED_FACE('',(#1133),#228,.T.);
#10586=ADVANCED_FACE('',(#1134),#10244,.T.);
#10587=ADVANCED_FACE('',(#1135),#699,.F.);
#10588=ADVANCED_FACE('',(#1136),#700,.T.);
#10589=ADVANCED_FACE('',(#1137),#701,.T.);
#10590=ADVANCED_FACE('',(#1138),#702,.T.);
#10591=ADVANCED_FACE('',(#1139),#703,.F.);
#10592=ADVANCED_FACE('',(#1140),#704,.T.);
#10593=ADVANCED_FACE('',(#1141),#705,.F.);
#10594=ADVANCED_FACE('',(#1142),#706,.F.);
#10595=ADVANCED_FACE('',(#1143),#707,.F.);
#10596=ADVANCED_FACE('',(#1144),#708,.T.);
#10597=ADVANCED_FACE('',(#1145),#709,.F.);
#10598=ADVANCED_FACE('',(#1146),#710,.T.);
#10599=ADVANCED_FACE('',(#1147),#711,.F.);
#10600=ADVANCED_FACE('',(#1148),#712,.F.);
#10601=ADVANCED_FACE('',(#1149),#713,.F.);
#10602=ADVANCED_FACE('',(#1150),#714,.T.);
#10603=ADVANCED_FACE('',(#1151),#715,.T.);
#10604=ADVANCED_FACE('',(#1152),#716,.T.);
#10605=ADVANCED_FACE('',(#1153),#717,.T.);
#10606=ADVANCED_FACE('',(#1154),#718,.T.);
#10607=ADVANCED_FACE('',(#1155),#719,.T.);
#10608=ADVANCED_FACE('',(#1156),#720,.F.);
#10609=ADVANCED_FACE('',(#1157),#721,.F.);
#10610=ADVANCED_FACE('',(#1158),#722,.F.);
#10611=ADVANCED_FACE('',(#1159),#723,.T.);
#10612=ADVANCED_FACE('',(#1160),#724,.F.);
#10613=ADVANCED_FACE('',(#1161),#725,.T.);
#10614=ADVANCED_FACE('',(#1162),#10245,.T.);
#10615=ADVANCED_FACE('',(#1163),#726,.F.);
#10616=ADVANCED_FACE('',(#1164),#727,.T.);
#10617=ADVANCED_FACE('',(#1165),#728,.T.);
#10618=ADVANCED_FACE('',(#1166),#729,.F.);
#10619=ADVANCED_FACE('',(#1167,#436),#730,.T.);
#10620=ADVANCED_FACE('',(#1168,#437),#731,.T.);
#10621=ADVANCED_FACE('',(#1169,#438),#732,.T.);
#10622=ADVANCED_FACE('',(#1170,#439),#733,.T.);
#10623=ADVANCED_FACE('',(#1171,#440),#734,.T.);
#10624=ADVANCED_FACE('',(#1172,#441),#735,.T.);
#10625=ADVANCED_FACE('',(#1173),#736,.F.);
#10626=ADVANCED_FACE('',(#1174),#737,.F.);
#10627=ADVANCED_FACE('',(#1175),#738,.F.);
#10628=ADVANCED_FACE('',(#1176),#739,.F.);
#10629=ADVANCED_FACE('',(#1177),#740,.T.);
#10630=ADVANCED_FACE('',(#1178),#741,.F.);
#10631=ADVANCED_FACE('',(#1179),#742,.T.);
#10632=ADVANCED_FACE('',(#1180),#743,.F.);
#10633=ADVANCED_FACE('',(#1181),#744,.F.);
#10634=ADVANCED_FACE('',(#1182),#745,.F.);
#10635=ADVANCED_FACE('',(#1183),#746,.F.);
#10636=ADVANCED_FACE('',(#1184,#442),#747,.F.);
#10637=ADVANCED_FACE('',(#1185),#748,.F.);
#10638=ADVANCED_FACE('',(#1186),#749,.F.);
#10639=ADVANCED_FACE('',(#1187),#750,.F.);
#10640=ADVANCED_FACE('',(#1188),#751,.T.);
#10641=ADVANCED_FACE('',(#1189),#752,.T.);
#10642=ADVANCED_FACE('',(#1190),#753,.T.);
#10643=ADVANCED_FACE('',(#1191),#754,.T.);
#10644=ADVANCED_FACE('',(#1192,#443),#755,.F.);
#10645=ADVANCED_FACE('',(#1193),#756,.F.);
#10646=ADVANCED_FACE('',(#1194),#757,.T.);
#10647=ADVANCED_FACE('',(#1195),#758,.T.);
#10648=ADVANCED_FACE('',(#1196),#759,.T.);
#10649=ADVANCED_FACE('',(#1197),#760,.T.);
#10650=ADVANCED_FACE('',(#1198),#761,.F.);
#10651=ADVANCED_FACE('',(#1199),#762,.F.);
#10652=ADVANCED_FACE('',(#1200),#763,.F.);
#10653=ADVANCED_FACE('',(#1201),#764,.T.);
#10654=ADVANCED_FACE('',(#1202),#765,.T.);
#10655=ADVANCED_FACE('',(#1203),#766,.T.);
#10656=ADVANCED_FACE('',(#1204),#767,.T.);
#10657=ADVANCED_FACE('',(#1205),#768,.T.);
#10658=ADVANCED_FACE('',(#1206),#769,.T.);
#10659=ADVANCED_FACE('',(#1207),#770,.T.);
#10660=ADVANCED_FACE('',(#1208),#771,.T.);
#10661=ADVANCED_FACE('',(#1209),#772,.T.);
#10662=ADVANCED_FACE('',(#1210),#773,.T.);
#10663=ADVANCED_FACE('',(#1211),#774,.T.);
#10664=ADVANCED_FACE('',(#1212),#246,.T.);
#10665=ADVANCED_FACE('',(#1213),#247,.T.);
#10666=ADVANCED_FACE('',(#1214),#248,.T.);
#10667=ADVANCED_FACE('',(#1215),#249,.T.);
#10668=ADVANCED_FACE('',(#1216),#250,.T.);
#10669=ADVANCED_FACE('',(#1217),#251,.T.);
#10670=ADVANCED_FACE('',(#1218,#444),#775,.F.);
#10671=ADVANCED_FACE('',(#1219),#776,.F.);
#10672=ADVANCED_FACE('',(#1220),#777,.F.);
#10673=ADVANCED_FACE('',(#1221),#778,.F.);
#10674=ADVANCED_FACE('',(#1222),#779,.F.);
#10675=ADVANCED_FACE('',(#1223,#445),#780,.F.);
#10676=ADVANCED_FACE('',(#1224),#781,.F.);
#10677=ADVANCED_FACE('',(#1225),#782,.F.);
#10678=ADVANCED_FACE('',(#1226),#783,.F.);
#10679=ADVANCED_FACE('',(#1227),#784,.F.);
#10680=ADVANCED_FACE('',(#1228),#785,.F.);
#10681=ADVANCED_FACE('',(#1229),#786,.F.);
#10682=ADVANCED_FACE('',(#1230),#787,.F.);
#10683=ADVANCED_FACE('',(#1231),#788,.F.);
#10684=ADVANCED_FACE('',(#1232),#789,.T.);
#10685=ADVANCED_FACE('',(#1233),#790,.T.);
#10686=ADVANCED_FACE('',(#1234),#791,.F.);
#10687=ADVANCED_FACE('',(#1235),#792,.T.);
#10688=ADVANCED_FACE('',(#1236),#793,.T.);
#10689=ADVANCED_FACE('',(#1237),#794,.T.);
#10690=ADVANCED_FACE('',(#1238),#795,.T.);
#10691=ADVANCED_FACE('',(#1239),#234,.T.);
#10692=ADVANCED_FACE('',(#1240),#235,.T.);
#10693=ADVANCED_FACE('',(#1241),#236,.T.);
#10694=ADVANCED_FACE('',(#1242),#237,.T.);
#10695=ADVANCED_FACE('',(#1243),#238,.T.);
#10696=ADVANCED_FACE('',(#1244),#239,.T.);
#10697=ADVANCED_FACE('',(#1245),#796,.T.);
#10698=ADVANCED_FACE('',(#1246),#797,.T.);
#10699=ADVANCED_FACE('',(#1247),#798,.T.);
#10700=ADVANCED_FACE('',(#1248),#799,.T.);
#10701=ADVANCED_FACE('',(#1249),#800,.F.);
#10702=ADVANCED_FACE('',(#1250),#801,.T.);
#10703=ADVANCED_FACE('',(#1251,#446),#802,.F.);
#10704=ADVANCED_FACE('',(#1252),#803,.T.);
#10705=ADVANCED_FACE('',(#1253,#447),#804,.F.);
#10706=ADVANCED_FACE('',(#1254,#448),#805,.T.);
#10707=ADVANCED_FACE('',(#1255,#449),#806,.T.);
#10708=ADVANCED_FACE('',(#1256),#807,.T.);
#10709=ADVANCED_FACE('',(#1257),#10246,.F.);
#10710=ADVANCED_FACE('',(#1258),#10247,.F.);
#10711=ADVANCED_FACE('',(#1259),#10248,.F.);
#10712=ADVANCED_FACE('',(#1260),#10249,.F.);
#10713=ADVANCED_FACE('',(#1261),#10250,.F.);
#10714=ADVANCED_FACE('',(#1262),#10251,.F.);
#10715=ADVANCED_FACE('',(#1263),#10252,.F.);
#10716=ADVANCED_FACE('',(#1264),#10253,.F.);
#10717=ADVANCED_FACE('',(#1265),#10254,.F.);
#10718=ADVANCED_FACE('',(#1266),#10255,.F.);
#10719=ADVANCED_FACE('',(#1267),#10256,.F.);
#10720=ADVANCED_FACE('',(#1268),#10257,.F.);
#10721=ADVANCED_FACE('',(#1269),#10258,.F.);
#10722=ADVANCED_FACE('',(#1270),#10259,.F.);
#10723=ADVANCED_FACE('',(#1271),#10260,.F.);
#10724=ADVANCED_FACE('',(#1272),#10261,.F.);
#10725=ADVANCED_FACE('',(#1273),#10262,.F.);
#10726=ADVANCED_FACE('',(#1274),#10263,.F.);
#10727=ADVANCED_FACE('',(#1275),#10264,.F.);
#10728=ADVANCED_FACE('',(#1276),#10265,.F.);
#10729=ADVANCED_FACE('',(#1277),#10266,.F.);
#10730=ADVANCED_FACE('',(#1278),#10267,.F.);
#10731=ADVANCED_FACE('',(#1279),#10268,.F.);
#10732=ADVANCED_FACE('',(#1280),#10269,.F.);
#10733=ADVANCED_FACE('',(#1281),#10270,.F.);
#10734=ADVANCED_FACE('',(#1282),#205,.F.);
#10735=ADVANCED_FACE('',(#1283),#206,.F.);
#10736=ADVANCED_FACE('',(#1284),#207,.F.);
#10737=ADVANCED_FACE('',(#1285),#208,.F.);
#10738=ADVANCED_FACE('',(#1286),#209,.F.);
#10739=ADVANCED_FACE('',(#1287),#210,.F.);
#10740=ADVANCED_FACE('',(#1288),#211,.F.);
#10741=ADVANCED_FACE('',(#1289),#212,.F.);
#10742=ADVANCED_FACE('',(#1290),#213,.F.);
#10743=ADVANCED_FACE('',(#1291),#10271,.F.);
#10744=ADVANCED_FACE('',(#1292),#10272,.F.);
#10745=ADVANCED_FACE('',(#1293),#10273,.F.);
#10746=ADVANCED_FACE('',(#1294),#10274,.F.);
#10747=ADVANCED_FACE('',(#1295),#10275,.F.);
#10748=ADVANCED_FACE('',(#1296),#10276,.F.);
#10749=ADVANCED_FACE('',(#1297),#10277,.F.);
#10750=ADVANCED_FACE('',(#1298),#10278,.F.);
#10751=ADVANCED_FACE('',(#1299,#450,#451,#452,#453,#454,#455,#456,#457,
#458,#459,#460,#461,#462,#463,#464,#465,#466,#467,#468,#469,#470,#471,#472,
#473,#474),#808,.F.);
#10752=ADVANCED_FACE('',(#1300),#10279,.F.);
#10753=ADVANCED_FACE('',(#1301),#809,.F.);
#10754=ADVANCED_FACE('',(#1302),#10280,.F.);
#10755=ADVANCED_FACE('',(#1303),#10281,.F.);
#10756=ADVANCED_FACE('',(#1304),#810,.T.);
#10757=ADVANCED_FACE('',(#1305),#10282,.F.);
#10758=ADVANCED_FACE('',(#1306,#475,#476,#477,#478,#479,#480,#481,#482,
#483,#484,#485,#486,#487,#488,#489,#490,#491,#492,#493,#494,#495,#496,#497,
#498,#499),#811,.T.);
#10759=ADVANCED_FACE('',(#1307,#500,#501,#502,#503),#812,.F.);
#10760=ADVANCED_FACE('',(#1308),#240,.F.);
#10761=ADVANCED_FACE('',(#1309),#241,.F.);
#10762=ADVANCED_FACE('',(#1310,#504,#505,#506,#507),#813,.F.);
#10763=ADVANCED_FACE('',(#1311),#10283,.T.);
#10764=ADVANCED_FACE('',(#1312),#10284,.T.);
#10765=ADVANCED_FACE('',(#1313),#814,.T.);
#10766=ADVANCED_FACE('',(#1314),#10285,.T.);
#10767=ADVANCED_FACE('',(#1315),#10286,.T.);
#10768=ADVANCED_FACE('',(#1316),#815,.T.);
#10769=ADVANCED_FACE('',(#1317),#10287,.T.);
#10770=ADVANCED_FACE('',(#1318),#242,.F.);
#10771=ADVANCED_FACE('',(#1319),#243,.T.);
#10772=ADVANCED_FACE('',(#1320),#816,.F.);
#10773=ADVANCED_FACE('',(#1321),#10288,.T.);
#10774=ADVANCED_FACE('',(#1322),#10289,.T.);
#10775=ADVANCED_FACE('',(#1323),#817,.T.);
#10776=ADVANCED_FACE('',(#1324),#10290,.T.);
#10777=ADVANCED_FACE('',(#1325,#508,#509,#510,#511),#818,.T.);
#10778=ADVANCED_FACE('',(#1326,#512,#513,#514,#515),#819,.T.);
#10779=ADVANCED_FACE('',(#1327),#820,.T.);
#10780=ADVANCED_FACE('',(#1328),#821,.T.);
#10781=ADVANCED_FACE('',(#1329),#10291,.T.);
#10782=ADVANCED_FACE('',(#1330),#10292,.T.);
#10783=ADVANCED_FACE('',(#1331),#10293,.T.);
#10784=ADVANCED_FACE('',(#1332),#10294,.T.);
#10785=ADVANCED_FACE('',(#1333),#10295,.T.);
#10786=ADVANCED_FACE('',(#1334),#10296,.T.);
#10787=ADVANCED_FACE('',(#1335),#10297,.T.);
#10788=ADVANCED_FACE('',(#1336),#10298,.T.);
#10789=ADVANCED_FACE('',(#1337),#214,.F.);
#10790=ADVANCED_FACE('',(#1338),#10299,.F.);
#10791=ADVANCED_FACE('',(#1339),#10300,.F.);
#10792=ADVANCED_FACE('',(#1340),#10301,.F.);
#10793=ADVANCED_FACE('',(#1341),#10302,.F.);
#10794=ADVANCED_FACE('',(#1342),#10303,.F.);
#10795=ADVANCED_FACE('',(#1343),#10304,.F.);
#10796=ADVANCED_FACE('',(#1344),#10305,.F.);
#10797=ADVANCED_FACE('',(#1345),#10306,.F.);
#10798=ADVANCED_FACE('',(#1346),#10307,.F.);
#10799=ADVANCED_FACE('',(#1347),#10308,.F.);
#10800=ADVANCED_FACE('',(#1348,#516,#517,#518,#519,#520,#521,#522,#523,
#524,#525),#822,.T.);
#10801=ADVANCED_FACE('',(#1349,#526,#527,#528,#529,#530,#531,#532,#533,
#534,#535),#823,.F.);
#10802=ADVANCED_FACE('',(#1350),#10309,.T.);
#10803=ADVANCED_FACE('',(#1351),#10310,.T.);
#10804=ADVANCED_FACE('',(#1352),#824,.F.);
#10805=ADVANCED_FACE('',(#1353),#825,.T.);
#10806=ADVANCED_FACE('',(#1354),#10311,.F.);
#10807=ADVANCED_FACE('',(#1355),#10312,.F.);
#10808=ADVANCED_FACE('',(#1356),#10313,.F.);
#10809=ADVANCED_FACE('',(#1357),#10314,.T.);
#10810=ADVANCED_FACE('',(#1358),#10315,.F.);
#10811=ADVANCED_FACE('',(#1359),#10316,.F.);
#10812=ADVANCED_FACE('',(#1360,#536,#537,#538),#826,.F.);
#10813=ADVANCED_FACE('',(#1361),#827,.T.);
#10814=ADVANCED_FACE('',(#1362),#828,.F.);
#10815=ADVANCED_FACE('',(#1363),#829,.F.);
#10816=ADVANCED_FACE('',(#1364),#830,.F.);
#10817=ADVANCED_FACE('',(#1365,#539,#540,#541),#831,.F.);
#10818=ADVANCED_FACE('',(#1366),#832,.F.);
#10819=ADVANCED_FACE('',(#1367),#10317,.T.);
#10820=ADVANCED_FACE('',(#1368),#833,.F.);
#10821=ADVANCED_FACE('',(#1369),#834,.T.);
#10822=ADVANCED_FACE('',(#1370,#542,#543),#835,.F.);
#10823=ADVANCED_FACE('',(#1371,#544,#545),#836,.F.);
#10824=ADVANCED_FACE('',(#1372),#10318,.F.);
#10825=ADVANCED_FACE('',(#1373),#837,.F.);
#10826=ADVANCED_FACE('',(#1374),#838,.F.);
#10827=ADVANCED_FACE('',(#1375),#839,.F.);
#10828=ADVANCED_FACE('',(#1376),#10319,.F.);
#10829=ADVANCED_FACE('',(#1377),#10320,.F.);
#10830=ADVANCED_FACE('',(#1378),#840,.F.);
#10831=ADVANCED_FACE('',(#1379),#841,.F.);
#10832=ADVANCED_FACE('',(#1380),#842,.F.);
#10833=ADVANCED_FACE('',(#1381),#843,.F.);
#10834=ADVANCED_FACE('',(#1382),#844,.T.);
#10835=ADVANCED_FACE('',(#1383),#845,.F.);
#10836=ADVANCED_FACE('',(#1384),#10321,.F.);
#10837=ADVANCED_FACE('',(#1385),#10322,.F.);
#10838=ADVANCED_FACE('',(#1386),#10323,.F.);
#10839=ADVANCED_FACE('',(#1387),#10324,.F.);
#10840=ADVANCED_FACE('',(#1388),#10325,.F.);
#10841=ADVANCED_FACE('',(#1389),#846,.F.);
#10842=ADVANCED_FACE('',(#1390,#546,#547),#847,.F.);
#10843=ADVANCED_FACE('',(#1391),#848,.F.);
#10844=ADVANCED_FACE('',(#1392,#548,#549),#849,.F.);
#10845=ADVANCED_FACE('',(#1393),#850,.F.);
#10846=ADVANCED_FACE('',(#1394,#550,#551),#851,.F.);
#10847=ADVANCED_FACE('',(#1395,#552,#553),#852,.F.);
#10848=ADVANCED_FACE('',(#1396),#853,.T.);
#10849=ADVANCED_FACE('',(#1397),#854,.F.);
#10850=ADVANCED_FACE('',(#1398),#855,.T.);
#10851=ADVANCED_FACE('',(#1399),#856,.F.);
#10852=ADVANCED_FACE('',(#1400),#857,.T.);
#10853=ADVANCED_FACE('',(#1401),#858,.F.);
#10854=ADVANCED_FACE('',(#1402),#10326,.T.);
#10855=ADVANCED_FACE('',(#1403),#859,.T.);
#10856=ADVANCED_FACE('',(#1404),#860,.T.);
#10857=ADVANCED_FACE('',(#1405),#10327,.F.);
#10858=ADVANCED_FACE('',(#1406),#10328,.F.);
#10859=ADVANCED_FACE('',(#1407,#554),#861,.F.);
#10860=ADVANCED_FACE('',(#1408),#862,.F.);
#10861=ADVANCED_FACE('',(#1409,#555),#863,.F.);
#10862=ADVANCED_FACE('',(#1410),#864,.F.);
#10863=ADVANCED_FACE('',(#1411),#865,.F.);
#10864=ADVANCED_FACE('',(#1412),#866,.F.);
#10865=ADVANCED_FACE('',(#1413),#229,.F.);
#10866=ADVANCED_FACE('',(#1414),#215,.F.);
#10867=ADVANCED_FACE('',(#1415),#10329,.F.);
#10868=ADVANCED_FACE('',(#1416),#216,.F.);
#10869=ADVANCED_FACE('',(#1417),#10330,.T.);
#10870=ADVANCED_FACE('',(#1418),#10331,.T.);
#10871=ADVANCED_FACE('',(#1419,#556),#867,.F.);
#10872=ADVANCED_FACE('',(#1420,#557),#868,.F.);
#10873=ADVANCED_FACE('',(#1421),#252,.T.);
#10874=ADVANCED_FACE('',(#1422),#253,.T.);
#10875=ADVANCED_FACE('',(#1423),#254,.T.);
#10876=ADVANCED_FACE('',(#1424),#255,.T.);
#10877=ADVANCED_FACE('',(#1425),#256,.T.);
#10878=ADVANCED_FACE('',(#1426),#257,.T.);
#10879=ADVANCED_FACE('',(#1427),#258,.T.);
#10880=ADVANCED_FACE('',(#1428),#259,.T.);
#10881=ADVANCED_FACE('',(#1429),#260,.T.);
#10882=ADVANCED_FACE('',(#1430),#261,.T.);
#10883=ADVANCED_FACE('',(#1431),#262,.T.);
#10884=ADVANCED_FACE('',(#1432),#263,.T.);
#10885=ADVANCED_FACE('',(#1433),#10332,.T.);
#10886=ADVANCED_FACE('',(#1434),#10333,.F.);
#10887=ADVANCED_FACE('',(#1435,#558),#869,.F.);
#10888=ADVANCED_FACE('',(#1436,#559),#870,.F.);
#10889=ADVANCED_FACE('',(#1437),#10334,.T.);
#10890=ADVANCED_FACE('',(#1438),#10335,.F.);
#10891=ADVANCED_FACE('',(#1439,#560),#871,.F.);
#10892=ADVANCED_FACE('',(#1440,#561),#872,.F.);
#10893=ADVANCED_FACE('',(#1441),#10336,.T.);
#10894=ADVANCED_FACE('',(#1442),#10337,.F.);
#10895=ADVANCED_FACE('',(#1443),#230,.F.);
#10896=ADVANCED_FACE('',(#1444),#10338,.F.);
#10897=ADVANCED_FACE('',(#1445),#10339,.T.);
#10898=ADVANCED_FACE('',(#1446),#217,.T.);
#10899=ADVANCED_FACE('',(#1447,#562),#873,.F.);
#10900=ADVANCED_FACE('',(#1448,#563),#874,.F.);
#10901=ADVANCED_FACE('',(#1449,#564),#875,.T.);
#10902=ADVANCED_FACE('',(#1450),#10340,.T.);
#10903=ADVANCED_FACE('',(#1451),#10341,.F.);
#10904=ADVANCED_FACE('',(#1452),#10342,.T.);
#10905=ADVANCED_FACE('',(#1453,#565),#876,.T.);
#10906=ADVANCED_FACE('',(#1454,#566),#877,.F.);
#10907=ADVANCED_FACE('',(#1455,#567),#878,.F.);
#10908=ADVANCED_FACE('',(#1456),#10343,.T.);
#10909=ADVANCED_FACE('',(#1457),#10344,.F.);
#10910=ADVANCED_FACE('',(#1458),#10345,.T.);
#10911=ADVANCED_FACE('',(#1459,#568),#879,.T.);
#10912=ADVANCED_FACE('',(#1460,#569),#880,.F.);
#10913=ADVANCED_FACE('',(#1461,#570),#881,.F.);
#10914=ADVANCED_FACE('',(#1462),#218,.F.);
#10915=ADVANCED_FACE('',(#1463),#10346,.F.);
#10916=ADVANCED_FACE('',(#1464),#219,.F.);
#10917=ADVANCED_FACE('',(#1465),#10347,.F.);
#10918=ADVANCED_FACE('',(#1466),#10348,.T.);
#10919=ADVANCED_FACE('',(#1467,#571,#572),#882,.T.);
#10920=ADVANCED_FACE('',(#1468,#573,#574),#883,.F.);
#10921=ADVANCED_FACE('',(#1469),#10349,.T.);
#10922=ADVANCED_FACE('',(#1470),#884,.F.);
#10923=ADVANCED_FACE('',(#1471),#885,.F.);
#10924=ADVANCED_FACE('',(#1472),#220,.F.);
#10925=ADVANCED_FACE('',(#1473),#231,.F.);
#10926=ADVANCED_FACE('',(#1474),#10350,.T.);
#10927=ADVANCED_FACE('',(#1475),#221,.T.);
#10928=ADVANCED_FACE('',(#1476),#10351,.T.);
#10929=ADVANCED_FACE('',(#1477),#222,.T.);
#10930=ADVANCED_FACE('',(#1478,#575),#886,.T.);
#10931=ADVANCED_FACE('',(#1479),#887,.T.);
#10932=ADVANCED_FACE('',(#1480),#888,.T.);
#10933=ADVANCED_FACE('',(#1481),#889,.T.);
#10934=ADVANCED_FACE('',(#1482),#890,.T.);
#10935=ADVANCED_FACE('',(#1483),#891,.T.);
#10936=ADVANCED_FACE('',(#1484),#892,.T.);
#10937=ADVANCED_FACE('',(#1485),#893,.T.);
#10938=ADVANCED_FACE('',(#1486),#894,.T.);
#10939=ADVANCED_FACE('',(#1487),#895,.T.);
#10940=ADVANCED_FACE('',(#1488),#896,.T.);
#10941=ADVANCED_FACE('',(#1489),#897,.T.);
#10942=ADVANCED_FACE('',(#1490),#898,.T.);
#10943=ADVANCED_FACE('',(#1491),#899,.T.);
#10944=CLOSED_SHELL('',(#10352,#10353,#10354,#10355,#10356,#10357,#10358,
#10359,#10360,#10361,#10362,#10363,#10364,#10365,#10366,#10367,#10368,#10369,
#10370,#10371,#10372,#10373,#10374,#10375,#10376,#10377,#10378,#10379,#10380,
#10381,#10382,#10383,#10384,#10385,#10386,#10387,#10388,#10389,#10390,#10391,
#10392,#10393,#10394,#10395,#10396,#10397,#10398,#10399,#10400,#10401,#10402));
#10945=CLOSED_SHELL('',(#10403,#10404,#10405,#10406,#10407,#10408,#10409,
#10410,#10411,#10412,#10413,#10414,#10415,#10416,#10417,#10418,#10419,#10420,
#10421,#10422,#10423,#10424,#10425,#10426,#10427,#10428,#10429,#10430,#10431,
#10432,#10433,#10434,#10435,#10436,#10437,#10438,#10439,#10440,#10441,#10442,
#10443,#10444,#10445,#10446,#10447,#10448,#10449,#10450,#10451,#10452,#10453,
#10454,#10455,#10456,#10457,#10458,#10459,#10460,#10461,#10462,#10463,#10464,
#10465,#10466,#10467,#10468,#10469,#10470,#10471,#10472,#10473,#10474,#10475,
#10476,#10477,#10478,#10479,#10480,#10481,#10482,#10483,#10484,#10485,#10486,
#10487,#10488,#10489,#10490,#10491,#10492,#10493,#10494,#10495,#10496,#10497,
#10498,#10499,#10500,#10501,#10502,#10503,#10504,#10505,#10506,#10507,#10508,
#10509,#10510,#10511,#10512,#10513,#10514,#10515,#10516,#10517,#10518,#10519,
#10520,#10521,#10522,#10523,#10524,#10525,#10526,#10527,#10528,#10529,#10530,
#10531,#10532,#10533,#10534,#10535,#10536,#10537,#10538,#10539,#10540,#10541,
#10542,#10543,#10544,#10545,#10546,#10547,#10548,#10549,#10550,#10551,#10552,
#10553,#10554,#10555,#10556,#10557,#10558,#10559,#10560,#10561,#10562,#10563,
#10564,#10565,#10566,#10567,#10568,#10569,#10570,#10571,#10572,#10573,#10574,
#10575,#10576,#10577,#10578,#10579,#10580,#10581,#10582,#10583,#10584,#10585,
#10586,#10587,#10588,#10589,#10590,#10591,#10592,#10593,#10594,#10595,#10596,
#10597,#10598,#10599,#10600,#10601,#10602,#10603,#10604,#10605,#10606,#10607,
#10608,#10609,#10610,#10611,#10612,#10613,#10614,#10615,#10616,#10617,#10618,
#10619,#10620,#10621,#10622,#10623,#10624,#10625,#10626,#10627,#10628,#10629,
#10630,#10631,#10632,#10633,#10634,#10635,#10636,#10637,#10638,#10639,#10640,
#10641,#10642,#10643,#10644,#10645,#10646,#10647,#10648,#10649,#10650,#10651,
#10652,#10653,#10654,#10655,#10656,#10657,#10658,#10659,#10660,#10661,#10662,
#10663,#10664,#10665,#10666,#10667,#10668,#10669,#10670,#10671,#10672,#10673,
#10674,#10675,#10676,#10677,#10678,#10679,#10680,#10681,#10682,#10683,#10684,
#10685,#10686,#10687,#10688,#10689,#10690,#10691,#10692,#10693,#10694,#10695,
#10696,#10697,#10698,#10699,#10700,#10701,#10702,#10703,#10704,#10705,#10706,
#10707,#10708));
#10946=CLOSED_SHELL('',(#10709,#10710,#10711,#10712,#10713,#10714,#10715,
#10716,#10717,#10718,#10719,#10720,#10721,#10722,#10723,#10724,#10725,#10726,
#10727,#10728,#10729,#10730,#10731,#10732,#10733,#10734,#10735,#10736,#10737,
#10738,#10739,#10740,#10741,#10742,#10743,#10744,#10745,#10746,#10747,#10748,
#10749,#10750,#10751,#10752,#10753,#10754,#10755,#10756,#10757,#10758,#10759,
#10760,#10761,#10762,#10763,#10764,#10765,#10766,#10767,#10768,#10769,#10770,
#10771,#10772,#10773,#10774,#10775,#10776,#10777,#10778,#10779,#10780));
#10947=CLOSED_SHELL('',(#10789,#10790,#10791,#10792,#10793,#10794,#10795,
#10796,#10797,#10798,#10799,#10800,#10801,#10802,#10803,#10804,#10805));
#10948=CLOSED_SHELL('',(#10806,#10807,#10808,#10809,#10810,#10811,#10812,
#10813,#10814,#10815,#10816,#10817,#10818,#10819,#10820,#10821,#10822,#10823,
#10824,#10825,#10826,#10827,#10828,#10829));
#10949=CLOSED_SHELL('',(#10830,#10831,#10832,#10833,#10834,#10835));
#10950=CLOSED_SHELL('',(#10836,#10837,#10838,#10839,#10840,#10841,#10842,
#10843,#10844,#10845,#10846,#10847,#10848,#10849,#10850,#10851,#10852,#10853,
#10854,#10855,#10856,#10857,#10858,#10859,#10860,#10861,#10862,#10863,#10864));
#10951=CLOSED_SHELL('',(#10865,#10866,#10867,#10868,#10869,#10870,#10871,
#10872));
#10952=CLOSED_SHELL('',(#10873));
#10953=CLOSED_SHELL('',(#10874));
#10954=CLOSED_SHELL('',(#10875));
#10955=CLOSED_SHELL('',(#10876));
#10956=CLOSED_SHELL('',(#10877));
#10957=CLOSED_SHELL('',(#10878));
#10958=CLOSED_SHELL('',(#10879));
#10959=CLOSED_SHELL('',(#10880));
#10960=CLOSED_SHELL('',(#10881));
#10961=CLOSED_SHELL('',(#10882));
#10962=CLOSED_SHELL('',(#10883));
#10963=CLOSED_SHELL('',(#10884));
#10964=CLOSED_SHELL('',(#10885,#10886,#10887,#10888));
#10965=CLOSED_SHELL('',(#10889,#10890,#10891,#10892));
#10966=CLOSED_SHELL('',(#10893,#10894,#10895,#10896,#10897,#10898,#10899,
#10900,#10901));
#10967=CLOSED_SHELL('',(#10902,#10903,#10904,#10905,#10906,#10907));
#10968=CLOSED_SHELL('',(#10908,#10909,#10910,#10911,#10912,#10913));
#10969=CLOSED_SHELL('',(#10914,#10915,#10916,#10917,#10918,#10919,#10920,
#10921,#10922,#10923));
#10970=CLOSED_SHELL('',(#10924,#10925,#10926,#10927,#10928,#10929,#10930,
#10931,#10932,#10933,#10934,#10935,#10936,#10937,#10938,#10939,#10940,#10941,
#10942,#10943));
#10971=DERIVED_UNIT_ELEMENT(#10995,1.);
#10972=DERIVED_UNIT_ELEMENT(#20178,-3.);
#10973=DERIVED_UNIT_ELEMENT(#10995,1.);
#10974=DERIVED_UNIT_ELEMENT(#20178,-3.);
#10975=DERIVED_UNIT_ELEMENT(#10995,1.);
#10976=DERIVED_UNIT_ELEMENT(#20178,-3.);
#10977=DERIVED_UNIT_ELEMENT(#10995,1.);
#10978=DERIVED_UNIT_ELEMENT(#20178,-3.);
#10979=DERIVED_UNIT_ELEMENT(#10995,1.);
#10980=DERIVED_UNIT_ELEMENT(#20178,-3.);
#10981=DERIVED_UNIT_ELEMENT(#10995,1.);
#10982=DERIVED_UNIT_ELEMENT(#20178,-3.);
#10983=DERIVED_UNIT_ELEMENT(#10995,1.);
#10984=DERIVED_UNIT_ELEMENT(#20178,-3.);
#10985=DERIVED_UNIT_ELEMENT(#10995,1.);
#10986=DERIVED_UNIT_ELEMENT(#20178,-3.);
#10987=DERIVED_UNIT_ELEMENT(#10995,1.);
#10988=DERIVED_UNIT_ELEMENT(#20178,-3.);
#10989=DERIVED_UNIT_ELEMENT(#10995,1.);
#10990=DERIVED_UNIT_ELEMENT(#20178,-3.);
#10991=DERIVED_UNIT_ELEMENT(#10995,1.);
#10992=DERIVED_UNIT_ELEMENT(#20178,-3.);
#10993=DERIVED_UNIT_ELEMENT(#10995,1.);
#10994=DERIVED_UNIT_ELEMENT(#20178,-3.);
#10995=(
MASS_UNIT()
NAMED_UNIT(*)
SI_UNIT(.KILO.,.GRAM.)
);
#10996=DERIVED_UNIT((#10971,#10972));
#10997=DERIVED_UNIT((#10973,#10974));
#10998=DERIVED_UNIT((#10975,#10976));
#10999=DERIVED_UNIT((#10977,#10978));
#11000=DERIVED_UNIT((#10979,#10980));
#11001=DERIVED_UNIT((#10981,#10982));
#11002=DERIVED_UNIT((#10983,#10984));
#11003=DERIVED_UNIT((#10985,#10986));
#11004=DERIVED_UNIT((#10987,#10988));
#11005=DERIVED_UNIT((#10989,#10990));
#11006=DERIVED_UNIT((#10991,#10992));
#11007=DERIVED_UNIT((#10993,#10994));
#11008=MEASURE_REPRESENTATION_ITEM('density measure',
POSITIVE_RATIO_MEASURE(7850.),#10996);
#11009=MEASURE_REPRESENTATION_ITEM('density measure',
POSITIVE_RATIO_MEASURE(7850.),#10997);
#11010=MEASURE_REPRESENTATION_ITEM('density measure',
POSITIVE_RATIO_MEASURE(7850.),#10998);
#11011=MEASURE_REPRESENTATION_ITEM('density measure',
POSITIVE_RATIO_MEASURE(7850.),#10999);
#11012=MEASURE_REPRESENTATION_ITEM('density measure',
POSITIVE_RATIO_MEASURE(7850.),#11000);
#11013=MEASURE_REPRESENTATION_ITEM('density measure',
POSITIVE_RATIO_MEASURE(7850.),#11001);
#11014=MEASURE_REPRESENTATION_ITEM('density measure',
POSITIVE_RATIO_MEASURE(7850.),#11002);
#11015=MEASURE_REPRESENTATION_ITEM('density measure',
POSITIVE_RATIO_MEASURE(7850.),#11003);
#11016=MEASURE_REPRESENTATION_ITEM('density measure',
POSITIVE_RATIO_MEASURE(7850.),#11004);
#11017=MEASURE_REPRESENTATION_ITEM('density measure',
POSITIVE_RATIO_MEASURE(7850.),#11005);
#11018=MEASURE_REPRESENTATION_ITEM('density measure',
POSITIVE_RATIO_MEASURE(7850.),#11006);
#11019=MEASURE_REPRESENTATION_ITEM('density measure',
POSITIVE_RATIO_MEASURE(7850.),#11007);
#11020=PROPERTY_DEFINITION_REPRESENTATION(#11080,#11044);
#11021=PROPERTY_DEFINITION_REPRESENTATION(#11081,#11045);
#11022=PROPERTY_DEFINITION_REPRESENTATION(#11082,#11046);
#11023=PROPERTY_DEFINITION_REPRESENTATION(#11083,#11047);
#11024=PROPERTY_DEFINITION_REPRESENTATION(#11084,#11048);
#11025=PROPERTY_DEFINITION_REPRESENTATION(#11085,#11049);
#11026=PROPERTY_DEFINITION_REPRESENTATION(#11086,#11050);
#11027=PROPERTY_DEFINITION_REPRESENTATION(#11087,#11051);
#11028=PROPERTY_DEFINITION_REPRESENTATION(#11088,#11052);
#11029=PROPERTY_DEFINITION_REPRESENTATION(#11089,#11053);
#11030=PROPERTY_DEFINITION_REPRESENTATION(#11090,#11054);
#11031=PROPERTY_DEFINITION_REPRESENTATION(#11091,#11055);
#11032=PROPERTY_DEFINITION_REPRESENTATION(#11092,#11056);
#11033=PROPERTY_DEFINITION_REPRESENTATION(#11093,#11057);
#11034=PROPERTY_DEFINITION_REPRESENTATION(#11094,#11058);
#11035=PROPERTY_DEFINITION_REPRESENTATION(#11095,#11059);
#11036=PROPERTY_DEFINITION_REPRESENTATION(#11096,#11060);
#11037=PROPERTY_DEFINITION_REPRESENTATION(#11097,#11061);
#11038=PROPERTY_DEFINITION_REPRESENTATION(#11098,#11062);
#11039=PROPERTY_DEFINITION_REPRESENTATION(#11099,#11063);
#11040=PROPERTY_DEFINITION_REPRESENTATION(#11100,#11064);
#11041=PROPERTY_DEFINITION_REPRESENTATION(#11101,#11065);
#11042=PROPERTY_DEFINITION_REPRESENTATION(#11102,#11066);
#11043=PROPERTY_DEFINITION_REPRESENTATION(#11103,#11067);
#11044=REPRESENTATION('material name',(#11068),#20162);
#11045=REPRESENTATION('density',(#11008),#20162);
#11046=REPRESENTATION('material name',(#11069),#20163);
#11047=REPRESENTATION('density',(#11009),#20163);
#11048=REPRESENTATION('material name',(#11070),#20164);
#11049=REPRESENTATION('density',(#11010),#20164);
#11050=REPRESENTATION('material name',(#11071),#20165);
#11051=REPRESENTATION('density',(#11011),#20165);
#11052=REPRESENTATION('material name',(#11072),#20167);
#11053=REPRESENTATION('density',(#11012),#20167);
#11054=REPRESENTATION('material name',(#11073),#20168);
#11055=REPRESENTATION('density',(#11013),#20168);
#11056=REPRESENTATION('material name',(#11074),#20170);
#11057=REPRESENTATION('density',(#11014),#20170);
#11058=REPRESENTATION('material name',(#11075),#20171);
#11059=REPRESENTATION('density',(#11015),#20171);
#11060=REPRESENTATION('material name',(#11076),#20172);
#11061=REPRESENTATION('density',(#11016),#20172);
#11062=REPRESENTATION('material name',(#11077),#20173);
#11063=REPRESENTATION('density',(#11017),#20173);
#11064=REPRESENTATION('material name',(#11078),#20174);
#11065=REPRESENTATION('density',(#11018),#20174);
#11066=REPRESENTATION('material name',(#11079),#20175);
#11067=REPRESENTATION('density',(#11019),#20175);
#11068=DESCRIPTIVE_REPRESENTATION_ITEM('Steel','Steel');
#11069=DESCRIPTIVE_REPRESENTATION_ITEM('Steel','Steel');
#11070=DESCRIPTIVE_REPRESENTATION_ITEM('Steel','Steel');
#11071=DESCRIPTIVE_REPRESENTATION_ITEM('Steel','Steel');
#11072=DESCRIPTIVE_REPRESENTATION_ITEM('Steel','Steel');
#11073=DESCRIPTIVE_REPRESENTATION_ITEM('Steel','Steel');
#11074=DESCRIPTIVE_REPRESENTATION_ITEM('Steel','Steel');
#11075=DESCRIPTIVE_REPRESENTATION_ITEM('Steel','Steel');
#11076=DESCRIPTIVE_REPRESENTATION_ITEM('Steel','Steel');
#11077=DESCRIPTIVE_REPRESENTATION_ITEM('Steel','Steel');
#11078=DESCRIPTIVE_REPRESENTATION_ITEM('Steel','Steel');
#11079=DESCRIPTIVE_REPRESENTATION_ITEM('Steel','Steel');
#11080=PROPERTY_DEFINITION('material property','material name',#20272);
#11081=PROPERTY_DEFINITION('material property','density of part',#20272);
#11082=PROPERTY_DEFINITION('material property','material name',#20273);
#11083=PROPERTY_DEFINITION('material property','density of part',#20273);
#11084=PROPERTY_DEFINITION('material property','material name',#20274);
#11085=PROPERTY_DEFINITION('material property','density of part',#20274);
#11086=PROPERTY_DEFINITION('material property','material name',#20275);
#11087=PROPERTY_DEFINITION('material property','density of part',#20275);
#11088=PROPERTY_DEFINITION('material property','material name',#20277);
#11089=PROPERTY_DEFINITION('material property','density of part',#20277);
#11090=PROPERTY_DEFINITION('material property','material name',#20278);
#11091=PROPERTY_DEFINITION('material property','density of part',#20278);
#11092=PROPERTY_DEFINITION('material property','material name',#20280);
#11093=PROPERTY_DEFINITION('material property','density of part',#20280);
#11094=PROPERTY_DEFINITION('material property','material name',#20281);
#11095=PROPERTY_DEFINITION('material property','density of part',#20281);
#11096=PROPERTY_DEFINITION('material property','material name',#20282);
#11097=PROPERTY_DEFINITION('material property','density of part',#20282);
#11098=PROPERTY_DEFINITION('material property','material name',#20283);
#11099=PROPERTY_DEFINITION('material property','density of part',#20283);
#11100=PROPERTY_DEFINITION('material property','material name',#20284);
#11101=PROPERTY_DEFINITION('material property','density of part',#20284);
#11102=PROPERTY_DEFINITION('material property','material name',#20285);
#11103=PROPERTY_DEFINITION('material property','density of part',#20285);
#11104=AXIS2_PLACEMENT_3D('',#15422,#12214,#12215);
#11105=AXIS2_PLACEMENT_3D('',#15423,#12216,#12217);
#11106=AXIS2_PLACEMENT_3D('',#15424,#12218,#12219);
#11107=AXIS2_PLACEMENT_3D('',#15426,#12220,#12221);
#11108=AXIS2_PLACEMENT_3D('',#15429,#12223,#12224);
#11109=AXIS2_PLACEMENT_3D('',#15430,#12225,#12226);
#11110=AXIS2_PLACEMENT_3D('',#15432,#12227,#12228);
#11111=AXIS2_PLACEMENT_3D('',#15435,#12230,#12231);
#11112=AXIS2_PLACEMENT_3D('',#15436,#12232,#12233);
#11113=AXIS2_PLACEMENT_3D('',#15438,#12234,#12235);
#11114=AXIS2_PLACEMENT_3D('',#15441,#12237,#12238);
#11115=AXIS2_PLACEMENT_3D('',#15442,#12239,#12240);
#11116=AXIS2_PLACEMENT_3D('',#15444,#12241,#12242);
#11117=AXIS2_PLACEMENT_3D('',#15447,#12244,#12245);
#11118=AXIS2_PLACEMENT_3D('',#15448,#12246,#12247);
#11119=AXIS2_PLACEMENT_3D('',#15450,#12248,#12249);
#11120=AXIS2_PLACEMENT_3D('',#15453,#12251,#12252);
#11121=AXIS2_PLACEMENT_3D('',#15454,#12253,#12254);
#11122=AXIS2_PLACEMENT_3D('',#15456,#12255,#12256);
#11123=AXIS2_PLACEMENT_3D('',#15459,#12258,#12259);
#11124=AXIS2_PLACEMENT_3D('',#15460,#12260,#12261);
#11125=AXIS2_PLACEMENT_3D('',#15462,#12262,#12263);
#11126=AXIS2_PLACEMENT_3D('',#15465,#12265,#12266);
#11127=AXIS2_PLACEMENT_3D('',#15466,#12267,#12268);
#11128=AXIS2_PLACEMENT_3D('',#15468,#12269,#12270);
#11129=AXIS2_PLACEMENT_3D('',#15471,#12272,#12273);
#11130=AXIS2_PLACEMENT_3D('',#15472,#12274,#12275);
#11131=AXIS2_PLACEMENT_3D('',#15474,#12276,#12277);
#11132=AXIS2_PLACEMENT_3D('',#15477,#12279,#12280);
#11133=AXIS2_PLACEMENT_3D('',#15478,#12281,#12282);
#11134=AXIS2_PLACEMENT_3D('',#15480,#12283,#12284);
#11135=AXIS2_PLACEMENT_3D('',#15483,#12286,#12287);
#11136=AXIS2_PLACEMENT_3D('',#15484,#12288,#12289);
#11137=AXIS2_PLACEMENT_3D('',#15486,#12290,#12291);
#11138=AXIS2_PLACEMENT_3D('',#15489,#12293,#12294);
#11139=AXIS2_PLACEMENT_3D('',#15490,#12295,#12296);
#11140=AXIS2_PLACEMENT_3D('',#15492,#12297,#12298);
#11141=AXIS2_PLACEMENT_3D('',#15495,#12300,#12301);
#11142=AXIS2_PLACEMENT_3D('',#15496,#12302,#12303);
#11143=AXIS2_PLACEMENT_3D('',#15498,#12304,#12305);
#11144=AXIS2_PLACEMENT_3D('',#15501,#12307,#12308);
#11145=AXIS2_PLACEMENT_3D('',#15502,#12309,#12310);
#11146=AXIS2_PLACEMENT_3D('',#15504,#12311,#12312);
#11147=AXIS2_PLACEMENT_3D('',#15507,#12314,#12315);
#11148=AXIS2_PLACEMENT_3D('',#15508,#12316,#12317);
#11149=AXIS2_PLACEMENT_3D('',#15510,#12318,#12319);
#11150=AXIS2_PLACEMENT_3D('',#15513,#12321,#12322);
#11151=AXIS2_PLACEMENT_3D('',#15514,#12323,#12324);
#11152=AXIS2_PLACEMENT_3D('',#15516,#12325,#12326);
#11153=AXIS2_PLACEMENT_3D('',#15519,#12328,#12329);
#11154=AXIS2_PLACEMENT_3D('',#15520,#12330,#12331);
#11155=AXIS2_PLACEMENT_3D('',#15522,#12332,#12333);
#11156=AXIS2_PLACEMENT_3D('',#15525,#12335,#12336);
#11157=AXIS2_PLACEMENT_3D('',#15526,#12337,#12338);
#11158=AXIS2_PLACEMENT_3D('',#15531,#12340,#12341);
#11159=AXIS2_PLACEMENT_3D('',#15534,#12343,#12344);
#11160=AXIS2_PLACEMENT_3D('',#15535,#12345,#12346);
#11161=AXIS2_PLACEMENT_3D('',#15541,#12350,#12351);
#11162=AXIS2_PLACEMENT_3D('',#15546,#12353,#12354);
#11163=AXIS2_PLACEMENT_3D('',#15549,#12356,#12357);
#11164=AXIS2_PLACEMENT_3D('',#15550,#12358,#12359);
#11165=AXIS2_PLACEMENT_3D('',#15556,#12363,#12364);
#11166=AXIS2_PLACEMENT_3D('',#15560,#12366,#12367);
#11167=AXIS2_PLACEMENT_3D('',#15561,#12368,#12369);
#11168=AXIS2_PLACEMENT_3D('',#15562,#12370,#12371);
#11169=AXIS2_PLACEMENT_3D('',#15568,#12375,#12376);
#11170=AXIS2_PLACEMENT_3D('',#15573,#12378,#12379);
#11171=AXIS2_PLACEMENT_3D('',#15576,#12381,#12382);
#11172=AXIS2_PLACEMENT_3D('',#15577,#12383,#12384);
#11173=AXIS2_PLACEMENT_3D('',#15580,#12387,#12388);
#11174=AXIS2_PLACEMENT_3D('',#15584,#12390,#12391);
#11175=AXIS2_PLACEMENT_3D('',#15589,#12394,#12395);
#11176=AXIS2_PLACEMENT_3D('',#15593,#12397,#12398);
#11177=AXIS2_PLACEMENT_3D('',#15596,#12400,#12401);
#11178=AXIS2_PLACEMENT_3D('',#15597,#12402,#12403);
#11179=AXIS2_PLACEMENT_3D('',#15603,#12407,#12408);
#11180=AXIS2_PLACEMENT_3D('',#15605,#12409,#12410);
#11181=AXIS2_PLACEMENT_3D('',#15608,#12412,#12413);
#11182=AXIS2_PLACEMENT_3D('',#15610,#12414,#12415);
#11183=AXIS2_PLACEMENT_3D('',#15614,#12417,#12418);
#11184=AXIS2_PLACEMENT_3D('',#15617,#12421,#12422);
#11185=AXIS2_PLACEMENT_3D('',#15619,#12424,#12425);
#11186=AXIS2_PLACEMENT_3D('',#15621,#12427,#12428);
#11187=AXIS2_PLACEMENT_3D('',#15623,#12430,#12431);
#11188=AXIS2_PLACEMENT_3D('',#15625,#12432,#12433);
#11189=AXIS2_PLACEMENT_3D('',#15629,#12435,#12436);
#11190=AXIS2_PLACEMENT_3D('',#15633,#12438,#12439);
#11191=AXIS2_PLACEMENT_3D('',#15637,#12441,#12442);
#11192=AXIS2_PLACEMENT_3D('',#15639,#12444,#12445);
#11193=AXIS2_PLACEMENT_3D('',#15645,#12449,#12450);
#11194=AXIS2_PLACEMENT_3D('',#15649,#12452,#12453);
#11195=AXIS2_PLACEMENT_3D('',#15654,#12456,#12457);
#11196=AXIS2_PLACEMENT_3D('',#15657,#12459,#12460);
#11197=AXIS2_PLACEMENT_3D('',#15658,#12461,#12462);
#11198=AXIS2_PLACEMENT_3D('',#15659,#12463,#12464);
#11199=AXIS2_PLACEMENT_3D('',#15661,#12466,#12467);
#11200=AXIS2_PLACEMENT_3D('',#15663,#12469,#12470);
#11201=AXIS2_PLACEMENT_3D('',#15664,#12471,#12472);
#11202=AXIS2_PLACEMENT_3D('',#15666,#12474,#12475);
#11203=AXIS2_PLACEMENT_3D('',#15668,#12477,#12478);
#11204=AXIS2_PLACEMENT_3D('',#15671,#12481,#12482);
#11205=AXIS2_PLACEMENT_3D('',#15674,#12485,#12486);
#11206=AXIS2_PLACEMENT_3D('',#15677,#12489,#12490);
#11207=AXIS2_PLACEMENT_3D('',#15680,#12493,#12494);
#11208=AXIS2_PLACEMENT_3D('',#15681,#12495,#12496);
#11209=AXIS2_PLACEMENT_3D('',#15682,#12497,#12498);
#11210=AXIS2_PLACEMENT_3D('',#15683,#12499,#12500);
#11211=AXIS2_PLACEMENT_3D('',#15684,#12501,#12502);
#11212=AXIS2_PLACEMENT_3D('',#15685,#12503,#12504);
#11213=AXIS2_PLACEMENT_3D('',#15686,#12505,#12506);
#11214=AXIS2_PLACEMENT_3D('',#15687,#12507,#12508);
#11215=AXIS2_PLACEMENT_3D('',#15688,#12509,#12510);
#11216=AXIS2_PLACEMENT_3D('',#15689,#12511,#12512);
#11217=AXIS2_PLACEMENT_3D('',#15691,#12513,#12514);
#11218=AXIS2_PLACEMENT_3D('',#15694,#12516,#12517);
#11219=AXIS2_PLACEMENT_3D('',#15695,#12518,#12519);
#11220=AXIS2_PLACEMENT_3D('',#15697,#12520,#12521);
#11221=AXIS2_PLACEMENT_3D('',#15700,#12523,#12524);
#11222=AXIS2_PLACEMENT_3D('',#15701,#12525,#12526);
#11223=AXIS2_PLACEMENT_3D('',#15703,#12527,#12528);
#11224=AXIS2_PLACEMENT_3D('',#15706,#12530,#12531);
#11225=AXIS2_PLACEMENT_3D('',#15707,#12532,#12533);
#11226=AXIS2_PLACEMENT_3D('',#15709,#12534,#12535);
#11227=AXIS2_PLACEMENT_3D('',#15712,#12537,#12538);
#11228=AXIS2_PLACEMENT_3D('',#15713,#12539,#12540);
#11229=AXIS2_PLACEMENT_3D('',#15715,#12541,#12542);
#11230=AXIS2_PLACEMENT_3D('',#15718,#12544,#12545);
#11231=AXIS2_PLACEMENT_3D('',#15719,#12546,#12547);
#11232=AXIS2_PLACEMENT_3D('',#15721,#12548,#12549);
#11233=AXIS2_PLACEMENT_3D('',#15724,#12551,#12552);
#11234=AXIS2_PLACEMENT_3D('',#15725,#12553,#12554);
#11235=AXIS2_PLACEMENT_3D('',#15727,#12555,#12556);
#11236=AXIS2_PLACEMENT_3D('',#15730,#12558,#12559);
#11237=AXIS2_PLACEMENT_3D('',#15731,#12560,#12561);
#11238=AXIS2_PLACEMENT_3D('',#15733,#12562,#12563);
#11239=AXIS2_PLACEMENT_3D('',#15736,#12565,#12566);
#11240=AXIS2_PLACEMENT_3D('',#15737,#12567,#12568);
#11241=AXIS2_PLACEMENT_3D('',#15739,#12569,#12570);
#11242=AXIS2_PLACEMENT_3D('',#15742,#12572,#12573);
#11243=AXIS2_PLACEMENT_3D('',#15743,#12574,#12575);
#11244=AXIS2_PLACEMENT_3D('',#15745,#12576,#12577);
#11245=AXIS2_PLACEMENT_3D('',#15748,#12579,#12580);
#11246=AXIS2_PLACEMENT_3D('',#15749,#12581,#12582);
#11247=AXIS2_PLACEMENT_3D('',#15751,#12583,#12584);
#11248=AXIS2_PLACEMENT_3D('',#15754,#12586,#12587);
#11249=AXIS2_PLACEMENT_3D('',#15755,#12588,#12589);
#11250=AXIS2_PLACEMENT_3D('',#15757,#12590,#12591);
#11251=AXIS2_PLACEMENT_3D('',#15760,#12593,#12594);
#11252=AXIS2_PLACEMENT_3D('',#15761,#12595,#12596);
#11253=AXIS2_PLACEMENT_3D('',#15763,#12597,#12598);
#11254=AXIS2_PLACEMENT_3D('',#15766,#12600,#12601);
#11255=AXIS2_PLACEMENT_3D('',#15767,#12602,#12603);
#11256=AXIS2_PLACEMENT_3D('',#15769,#12604,#12605);
#11257=AXIS2_PLACEMENT_3D('',#15772,#12607,#12608);
#11258=AXIS2_PLACEMENT_3D('',#15773,#12609,#12610);
#11259=AXIS2_PLACEMENT_3D('',#15775,#12611,#12612);
#11260=AXIS2_PLACEMENT_3D('',#15778,#12614,#12615);
#11261=AXIS2_PLACEMENT_3D('',#15779,#12616,#12617);
#11262=AXIS2_PLACEMENT_3D('',#15781,#12618,#12619);
#11263=AXIS2_PLACEMENT_3D('',#15784,#12621,#12622);
#11264=AXIS2_PLACEMENT_3D('',#15785,#12623,#12624);
#11265=AXIS2_PLACEMENT_3D('',#15787,#12625,#12626);
#11266=AXIS2_PLACEMENT_3D('',#15790,#12628,#12629);
#11267=AXIS2_PLACEMENT_3D('',#15791,#12630,#12631);
#11268=AXIS2_PLACEMENT_3D('',#15793,#12632,#12633);
#11269=AXIS2_PLACEMENT_3D('',#15796,#12635,#12636);
#11270=AXIS2_PLACEMENT_3D('',#15797,#12637,#12638);
#11271=AXIS2_PLACEMENT_3D('',#15799,#12639,#12640);
#11272=AXIS2_PLACEMENT_3D('',#15802,#12642,#12643);
#11273=AXIS2_PLACEMENT_3D('',#15803,#12644,#12645);
#11274=AXIS2_PLACEMENT_3D('',#15805,#12646,#12647);
#11275=AXIS2_PLACEMENT_3D('',#15808,#12649,#12650);
#11276=AXIS2_PLACEMENT_3D('',#15809,#12651,#12652);
#11277=AXIS2_PLACEMENT_3D('',#15811,#12653,#12654);
#11278=AXIS2_PLACEMENT_3D('',#15814,#12656,#12657);
#11279=AXIS2_PLACEMENT_3D('',#15815,#12658,#12659);
#11280=AXIS2_PLACEMENT_3D('',#15817,#12660,#12661);
#11281=AXIS2_PLACEMENT_3D('',#15820,#12663,#12664);
#11282=AXIS2_PLACEMENT_3D('',#15821,#12665,#12666);
#11283=AXIS2_PLACEMENT_3D('',#15830,#12671,#12672);
#11284=AXIS2_PLACEMENT_3D('',#15832,#12673,#12674);
#11285=AXIS2_PLACEMENT_3D('',#15835,#12676,#12677);
#11286=AXIS2_PLACEMENT_3D('',#15836,#12678,#12679);
#11287=AXIS2_PLACEMENT_3D('',#15840,#12681,#12682);
#11288=AXIS2_PLACEMENT_3D('',#15841,#12683,#12684);
#11289=AXIS2_PLACEMENT_3D('',#15842,#12685,#12686);
#11290=AXIS2_PLACEMENT_3D('',#15846,#12688,#12689);
#11291=AXIS2_PLACEMENT_3D('',#15847,#12690,#12691);
#11292=AXIS2_PLACEMENT_3D('',#15848,#12692,#12693);
#11293=AXIS2_PLACEMENT_3D('',#15850,#12694,#12695);
#11294=AXIS2_PLACEMENT_3D('',#15853,#12697,#12698);
#11295=AXIS2_PLACEMENT_3D('',#15854,#12699,#12700);
#11296=AXIS2_PLACEMENT_3D('',#15855,#12701,#12702);
#11297=AXIS2_PLACEMENT_3D('',#15905,#12720,#12721);
#11298=AXIS2_PLACEMENT_3D('',#15906,#12722,#12723);
#11299=AXIS2_PLACEMENT_3D('',#15923,#12724,#12725);
#11300=AXIS2_PLACEMENT_3D('',#15924,#12726,#12727);
#11301=AXIS2_PLACEMENT_3D('',#15925,#12728,#12729);
#11302=AXIS2_PLACEMENT_3D('',#15936,#12733,#12734);
#11303=AXIS2_PLACEMENT_3D('',#16118,#12735,#12736);
#11304=AXIS2_PLACEMENT_3D('',#16182,#12740,#12741);
#11305=AXIS2_PLACEMENT_3D('',#16237,#12742,#12743);
#11306=AXIS2_PLACEMENT_3D('',#16296,#12747,#12748);
#11307=AXIS2_PLACEMENT_3D('',#16300,#12750,#12751);
#11308=AXIS2_PLACEMENT_3D('',#16301,#12752,#12753);
#11309=AXIS2_PLACEMENT_3D('',#16302,#12754,#12755);
#11310=AXIS2_PLACEMENT_3D('',#16306,#12757,#12758);
#11311=AXIS2_PLACEMENT_3D('',#16307,#12759,#12760);
#11312=AXIS2_PLACEMENT_3D('',#16308,#12761,#12762);
#11313=AXIS2_PLACEMENT_3D('',#16312,#12764,#12765);
#11314=AXIS2_PLACEMENT_3D('',#16313,#12766,#12767);
#11315=AXIS2_PLACEMENT_3D('',#16314,#12768,#12769);
#11316=AXIS2_PLACEMENT_3D('',#16319,#12771,#12772);
#11317=AXIS2_PLACEMENT_3D('',#16323,#12774,#12775);
#11318=AXIS2_PLACEMENT_3D('',#16327,#12777,#12778);
#11319=AXIS2_PLACEMENT_3D('',#16331,#12780,#12781);
#11320=AXIS2_PLACEMENT_3D('',#16335,#12783,#12784);
#11321=AXIS2_PLACEMENT_3D('',#16338,#12786,#12787);
#11322=AXIS2_PLACEMENT_3D('',#16342,#12789,#12790);
#11323=AXIS2_PLACEMENT_3D('',#16346,#12792,#12793);
#11324=AXIS2_PLACEMENT_3D('',#16350,#12795,#12796);
#11325=AXIS2_PLACEMENT_3D('',#16354,#12798,#12799);
#11326=AXIS2_PLACEMENT_3D('',#16358,#12801,#12802);
#11327=AXIS2_PLACEMENT_3D('',#16362,#12804,#12805);
#11328=AXIS2_PLACEMENT_3D('',#16366,#12807,#12808);
#11329=AXIS2_PLACEMENT_3D('',#16370,#12810,#12811);
#11330=AXIS2_PLACEMENT_3D('',#16374,#12813,#12814);
#11331=AXIS2_PLACEMENT_3D('',#16378,#12816,#12817);
#11332=AXIS2_PLACEMENT_3D('',#16381,#12819,#12820);
#11333=AXIS2_PLACEMENT_3D('',#16383,#12821,#12822);
#11334=AXIS2_PLACEMENT_3D('',#16386,#12824,#12825);
#11335=AXIS2_PLACEMENT_3D('',#16387,#12826,#12827);
#11336=AXIS2_PLACEMENT_3D('',#16389,#12828,#12829);
#11337=AXIS2_PLACEMENT_3D('',#16391,#12830,#12831);
#11338=AXIS2_PLACEMENT_3D('',#16393,#12833,#12834);
#11339=AXIS2_PLACEMENT_3D('',#16395,#12835,#12836);
#11340=AXIS2_PLACEMENT_3D('',#16397,#12838,#12839);
#11341=AXIS2_PLACEMENT_3D('',#16399,#12840,#12841);
#11342=AXIS2_PLACEMENT_3D('',#16402,#12843,#12844);
#11343=AXIS2_PLACEMENT_3D('',#16403,#12845,#12846);
#11344=AXIS2_PLACEMENT_3D('',#16405,#12847,#12848);
#11345=AXIS2_PLACEMENT_3D('',#16408,#12850,#12851);
#11346=AXIS2_PLACEMENT_3D('',#16409,#12852,#12853);
#11347=AXIS2_PLACEMENT_3D('',#16410,#12854,#12855);
#11348=AXIS2_PLACEMENT_3D('',#16411,#12856,#12857);
#11349=AXIS2_PLACEMENT_3D('',#16412,#12858,#12859);
#11350=AXIS2_PLACEMENT_3D('',#16413,#12860,#12861);
#11351=AXIS2_PLACEMENT_3D('',#16416,#12862,#12863);
#11352=AXIS2_PLACEMENT_3D('',#16420,#12865,#12866);
#11353=AXIS2_PLACEMENT_3D('',#16422,#12868,#12869);
#11354=AXIS2_PLACEMENT_3D('',#16423,#12870,#12871);
#11355=AXIS2_PLACEMENT_3D('',#16427,#12873,#12874);
#11356=AXIS2_PLACEMENT_3D('',#16431,#12876,#12877);
#11357=AXIS2_PLACEMENT_3D('',#16435,#12879,#12880);
#11358=AXIS2_PLACEMENT_3D('',#16439,#12882,#12883);
#11359=AXIS2_PLACEMENT_3D('',#16441,#12885,#12886);
#11360=AXIS2_PLACEMENT_3D('',#16442,#12887,#12888);
#11361=AXIS2_PLACEMENT_3D('',#16487,#12889,#12890);
#11362=AXIS2_PLACEMENT_3D('',#16488,#12891,#12892);
#11363=AXIS2_PLACEMENT_3D('',#16533,#12893,#12894);
#11364=AXIS2_PLACEMENT_3D('',#16534,#12895,#12896);
#11365=AXIS2_PLACEMENT_3D('',#16546,#12903,#12904);
#11366=AXIS2_PLACEMENT_3D('',#16550,#12907,#12908);
#11367=AXIS2_PLACEMENT_3D('',#16626,#12947,#12948);
#11368=AXIS2_PLACEMENT_3D('',#16630,#12951,#12952);
#11369=AXIS2_PLACEMENT_3D('',#16640,#12958,#12959);
#11370=AXIS2_PLACEMENT_3D('',#16644,#12961,#12962);
#11371=AXIS2_PLACEMENT_3D('',#16646,#12964,#12965);
#11372=AXIS2_PLACEMENT_3D('',#16674,#12980,#12981);
#11373=AXIS2_PLACEMENT_3D('',#16676,#12982,#12983);
#11374=AXIS2_PLACEMENT_3D('',#16678,#12985,#12986);
#11375=AXIS2_PLACEMENT_3D('',#16682,#12989,#12990);
#11376=AXIS2_PLACEMENT_3D('',#16685,#12991,#12992);
#11377=AXIS2_PLACEMENT_3D('',#16687,#12993,#12994);
#11378=AXIS2_PLACEMENT_3D('',#16689,#12996,#12997);
#11379=AXIS2_PLACEMENT_3D('',#16690,#12998,#12999);
#11380=AXIS2_PLACEMENT_3D('',#16710,#13010,#13011);
#11381=AXIS2_PLACEMENT_3D('',#16712,#13012,#13013);
#11382=AXIS2_PLACEMENT_3D('',#16714,#13014,#13015);
#11383=AXIS2_PLACEMENT_3D('',#16716,#13017,#13018);
#11384=AXIS2_PLACEMENT_3D('',#16717,#13019,#13020);
#11385=AXIS2_PLACEMENT_3D('',#16721,#13023,#13024);
#11386=AXIS2_PLACEMENT_3D('',#16723,#13025,#13026);
#11387=AXIS2_PLACEMENT_3D('',#16725,#13028,#13029);
#11388=AXIS2_PLACEMENT_3D('',#16753,#13044,#13045);
#11389=AXIS2_PLACEMENT_3D('',#16754,#13046,#13047);
#11390=AXIS2_PLACEMENT_3D('',#16755,#13048,#13049);
#11391=AXIS2_PLACEMENT_3D('',#16757,#13050,#13051);
#11392=AXIS2_PLACEMENT_3D('',#16758,#13052,#13053);
#11393=AXIS2_PLACEMENT_3D('',#16759,#13054,#13055);
#11394=AXIS2_PLACEMENT_3D('',#16763,#13058,#13059);
#11395=AXIS2_PLACEMENT_3D('',#16766,#13061,#13062);
#11396=AXIS2_PLACEMENT_3D('',#16767,#13063,#13064);
#11397=AXIS2_PLACEMENT_3D('',#16776,#13067,#13068);
#11398=AXIS2_PLACEMENT_3D('',#16778,#13069,#13070);
#11399=AXIS2_PLACEMENT_3D('',#16780,#13072,#13073);
#11400=AXIS2_PLACEMENT_3D('',#16794,#13076,#13077);
#11401=AXIS2_PLACEMENT_3D('',#16796,#13078,#13079);
#11402=AXIS2_PLACEMENT_3D('',#16798,#13081,#13082);
#11403=AXIS2_PLACEMENT_3D('',#16807,#13085,#13086);
#11404=AXIS2_PLACEMENT_3D('',#16810,#13088,#13089);
#11405=AXIS2_PLACEMENT_3D('',#16811,#13090,#13091);
#11406=AXIS2_PLACEMENT_3D('',#16820,#13094,#13095);
#11407=AXIS2_PLACEMENT_3D('',#16822,#13096,#13097);
#11408=AXIS2_PLACEMENT_3D('',#16824,#13099,#13100);
#11409=AXIS2_PLACEMENT_3D('',#16838,#13103,#13104);
#11410=AXIS2_PLACEMENT_3D('',#16840,#13105,#13106);
#11411=AXIS2_PLACEMENT_3D('',#16842,#13108,#13109);
#11412=AXIS2_PLACEMENT_3D('',#16851,#13112,#13113);
#11413=AXIS2_PLACEMENT_3D('',#16854,#13115,#13116);
#11414=AXIS2_PLACEMENT_3D('',#16855,#13117,#13118);
#11415=AXIS2_PLACEMENT_3D('',#16864,#13121,#13122);
#11416=AXIS2_PLACEMENT_3D('',#16866,#13123,#13124);
#11417=AXIS2_PLACEMENT_3D('',#16868,#13126,#13127);
#11418=AXIS2_PLACEMENT_3D('',#16882,#13130,#13131);
#11419=AXIS2_PLACEMENT_3D('',#16884,#13132,#13133);
#11420=AXIS2_PLACEMENT_3D('',#16886,#13135,#13136);
#11421=AXIS2_PLACEMENT_3D('',#16895,#13139,#13140);
#11422=AXIS2_PLACEMENT_3D('',#16898,#13142,#13143);
#11423=AXIS2_PLACEMENT_3D('',#16899,#13144,#13145);
#11424=AXIS2_PLACEMENT_3D('',#16902,#13147,#13148);
#11425=AXIS2_PLACEMENT_3D('',#16903,#13149,#13150);
#11426=AXIS2_PLACEMENT_3D('',#16904,#13151,#13152);
#11427=AXIS2_PLACEMENT_3D('',#16905,#13153,#13154);
#11428=AXIS2_PLACEMENT_3D('',#16915,#13160,#13161);
#11429=AXIS2_PLACEMENT_3D('',#16918,#13162,#13163);
#11430=AXIS2_PLACEMENT_3D('',#16926,#13167,#13168);
#11431=AXIS2_PLACEMENT_3D('',#16934,#13172,#13173);
#11432=AXIS2_PLACEMENT_3D('',#16942,#13177,#13178);
#11433=AXIS2_PLACEMENT_3D('',#16945,#13181,#13182);
#11434=AXIS2_PLACEMENT_3D('',#16949,#13185,#13186);
#11435=AXIS2_PLACEMENT_3D('',#16955,#13190,#13191);
#11436=AXIS2_PLACEMENT_3D('',#17028,#13229,#13230);
#11437=AXIS2_PLACEMENT_3D('',#17038,#13236,#13237);
#11438=AXIS2_PLACEMENT_3D('',#17068,#13253,#13254);
#11439=AXIS2_PLACEMENT_3D('',#17071,#13256,#13257);
#11440=AXIS2_PLACEMENT_3D('',#17072,#13258,#13259);
#11441=AXIS2_PLACEMENT_3D('',#17076,#13262,#13263);
#11442=AXIS2_PLACEMENT_3D('',#17080,#13265,#13266);
#11443=AXIS2_PLACEMENT_3D('',#17081,#13267,#13268);
#11444=AXIS2_PLACEMENT_3D('',#17082,#13269,#13270);
#11445=AXIS2_PLACEMENT_3D('',#17083,#13271,#13272);
#11446=AXIS2_PLACEMENT_3D('',#17103,#13283,#13284);
#11447=AXIS2_PLACEMENT_3D('',#17106,#13286,#13287);
#11448=AXIS2_PLACEMENT_3D('',#17108,#13288,#13289);
#11449=AXIS2_PLACEMENT_3D('',#17109,#13290,#13291);
#11450=AXIS2_PLACEMENT_3D('',#17110,#13292,#13293);
#11451=AXIS2_PLACEMENT_3D('',#17114,#13296,#13297);
#11452=AXIS2_PLACEMENT_3D('',#17117,#13299,#13300);
#11453=AXIS2_PLACEMENT_3D('',#17118,#13301,#13302);
#11454=AXIS2_PLACEMENT_3D('',#17146,#13317,#13318);
#11455=AXIS2_PLACEMENT_3D('',#17147,#13319,#13320);
#11456=AXIS2_PLACEMENT_3D('',#17148,#13321,#13322);
#11457=AXIS2_PLACEMENT_3D('',#17149,#13323,#13324);
#11458=AXIS2_PLACEMENT_3D('',#17150,#13325,#13326);
#11459=AXIS2_PLACEMENT_3D('',#17156,#13330,#13331);
#11460=AXIS2_PLACEMENT_3D('',#17159,#13334,#13335);
#11461=AXIS2_PLACEMENT_3D('',#17160,#13336,#13337);
#11462=AXIS2_PLACEMENT_3D('',#17165,#13341,#13342);
#11463=AXIS2_PLACEMENT_3D('',#17171,#13345,#13346);
#11464=AXIS2_PLACEMENT_3D('',#17173,#13348,#13349);
#11465=AXIS2_PLACEMENT_3D('',#17176,#13351,#13352);
#11466=AXIS2_PLACEMENT_3D('',#17177,#13353,#13354);
#11467=AXIS2_PLACEMENT_3D('',#17185,#13359,#13360);
#11468=AXIS2_PLACEMENT_3D('',#17188,#13363,#13364);
#11469=AXIS2_PLACEMENT_3D('',#17189,#13365,#13366);
#11470=AXIS2_PLACEMENT_3D('',#17195,#13370,#13371);
#11471=AXIS2_PLACEMENT_3D('',#17199,#13374,#13375);
#11472=AXIS2_PLACEMENT_3D('',#17205,#13379,#13380);
#11473=AXIS2_PLACEMENT_3D('',#17209,#13383,#13384);
#11474=AXIS2_PLACEMENT_3D('',#17213,#13387,#13388);
#11475=AXIS2_PLACEMENT_3D('',#17219,#13392,#13393);
#11476=AXIS2_PLACEMENT_3D('',#17226,#13398,#13399);
#11477=AXIS2_PLACEMENT_3D('',#17230,#13402,#13403);
#11478=AXIS2_PLACEMENT_3D('',#17235,#13407,#13408);
#11479=AXIS2_PLACEMENT_3D('',#17237,#13410,#13411);
#11480=AXIS2_PLACEMENT_3D('',#17239,#13413,#13414);
#11481=AXIS2_PLACEMENT_3D('',#17241,#13416,#13417);
#11482=AXIS2_PLACEMENT_3D('',#17245,#13420,#13421);
#11483=AXIS2_PLACEMENT_3D('',#17249,#13424,#13425);
#11484=AXIS2_PLACEMENT_3D('',#17254,#13429,#13430);
#11485=AXIS2_PLACEMENT_3D('',#17255,#13431,#13432);
#11486=AXIS2_PLACEMENT_3D('',#17259,#13435,#13436);
#11487=AXIS2_PLACEMENT_3D('',#17264,#13440,#13441);
#11488=AXIS2_PLACEMENT_3D('',#17266,#13443,#13444);
#11489=AXIS2_PLACEMENT_3D('',#17268,#13446,#13447);
#11490=AXIS2_PLACEMENT_3D('',#17270,#13449,#13450);
#11491=AXIS2_PLACEMENT_3D('',#17274,#13453,#13454);
#11492=AXIS2_PLACEMENT_3D('',#17278,#13457,#13458);
#11493=AXIS2_PLACEMENT_3D('',#17283,#13462,#13463);
#11494=AXIS2_PLACEMENT_3D('',#17285,#13465,#13466);
#11495=AXIS2_PLACEMENT_3D('',#17286,#13467,#13468);
#11496=AXIS2_PLACEMENT_3D('',#17287,#13469,#13470);
#11497=AXIS2_PLACEMENT_3D('',#17291,#13473,#13474);
#11498=AXIS2_PLACEMENT_3D('',#17299,#13479,#13480);
#11499=AXIS2_PLACEMENT_3D('',#17307,#13485,#13486);
#11500=AXIS2_PLACEMENT_3D('',#17315,#13491,#13492);
#11501=AXIS2_PLACEMENT_3D('',#17323,#13497,#13498);
#11502=AXIS2_PLACEMENT_3D('',#17331,#13503,#13504);
#11503=AXIS2_PLACEMENT_3D('',#17337,#13508,#13509);
#11504=AXIS2_PLACEMENT_3D('',#17341,#13512,#13513);
#11505=AXIS2_PLACEMENT_3D('',#17344,#13516,#13517);
#11506=AXIS2_PLACEMENT_3D('',#17346,#13519,#13520);
#11507=AXIS2_PLACEMENT_3D('',#17348,#13522,#13523);
#11508=AXIS2_PLACEMENT_3D('',#17352,#13526,#13527);
#11509=AXIS2_PLACEMENT_3D('',#17356,#13530,#13531);
#11510=AXIS2_PLACEMENT_3D('',#17362,#13535,#13536);
#11511=AXIS2_PLACEMENT_3D('',#17366,#13539,#13540);
#11512=AXIS2_PLACEMENT_3D('',#17368,#13542,#13543);
#11513=AXIS2_PLACEMENT_3D('',#17372,#13546,#13547);
#11514=AXIS2_PLACEMENT_3D('',#17378,#13551,#13552);
#11515=AXIS2_PLACEMENT_3D('',#17382,#13555,#13556);
#11516=AXIS2_PLACEMENT_3D('',#17386,#13559,#13560);
#11517=AXIS2_PLACEMENT_3D('',#17390,#13563,#13564);
#11518=AXIS2_PLACEMENT_3D('',#17392,#13566,#13567);
#11519=AXIS2_PLACEMENT_3D('',#17394,#13569,#13570);
#11520=AXIS2_PLACEMENT_3D('',#17396,#13572,#13573);
#11521=AXIS2_PLACEMENT_3D('',#17398,#13575,#13576);
#11522=AXIS2_PLACEMENT_3D('',#17399,#13577,#13578);
#11523=AXIS2_PLACEMENT_3D('',#17400,#13579,#13580);
#11524=AXIS2_PLACEMENT_3D('',#17401,#13581,#13582);
#11525=AXIS2_PLACEMENT_3D('',#17402,#13583,#13584);
#11526=AXIS2_PLACEMENT_3D('',#17403,#13585,#13586);
#11527=AXIS2_PLACEMENT_3D('',#17404,#13587,#13588);
#11528=AXIS2_PLACEMENT_3D('',#17405,#13589,#13590);
#11529=AXIS2_PLACEMENT_3D('',#17406,#13591,#13592);
#11530=AXIS2_PLACEMENT_3D('',#17407,#13593,#13594);
#11531=AXIS2_PLACEMENT_3D('',#17408,#13595,#13596);
#11532=AXIS2_PLACEMENT_3D('',#17409,#13597,#13598);
#11533=AXIS2_PLACEMENT_3D('',#17410,#13599,#13600);
#11534=AXIS2_PLACEMENT_3D('',#17411,#13601,#13602);
#11535=AXIS2_PLACEMENT_3D('',#17412,#13603,#13604);
#11536=AXIS2_PLACEMENT_3D('',#17413,#13605,#13606);
#11537=AXIS2_PLACEMENT_3D('',#17414,#13607,#13608);
#11538=AXIS2_PLACEMENT_3D('',#17415,#13609,#13610);
#11539=AXIS2_PLACEMENT_3D('',#17416,#13611,#13612);
#11540=AXIS2_PLACEMENT_3D('',#17417,#13613,#13614);
#11541=AXIS2_PLACEMENT_3D('',#17418,#13615,#13616);
#11542=AXIS2_PLACEMENT_3D('',#17419,#13617,#13618);
#11543=AXIS2_PLACEMENT_3D('',#17420,#13619,#13620);
#11544=AXIS2_PLACEMENT_3D('',#17421,#13621,#13622);
#11545=AXIS2_PLACEMENT_3D('',#17422,#13623,#13624);
#11546=AXIS2_PLACEMENT_3D('',#17423,#13625,#13626);
#11547=AXIS2_PLACEMENT_3D('',#17424,#13627,#13628);
#11548=AXIS2_PLACEMENT_3D('',#17425,#13629,#13630);
#11549=AXIS2_PLACEMENT_3D('',#17426,#13631,#13632);
#11550=AXIS2_PLACEMENT_3D('',#17427,#13633,#13634);
#11551=AXIS2_PLACEMENT_3D('',#17428,#13635,#13636);
#11552=AXIS2_PLACEMENT_3D('',#17429,#13637,#13638);
#11553=AXIS2_PLACEMENT_3D('',#17430,#13639,#13640);
#11554=AXIS2_PLACEMENT_3D('',#17431,#13641,#13642);
#11555=AXIS2_PLACEMENT_3D('',#17432,#13643,#13644);
#11556=AXIS2_PLACEMENT_3D('',#17433,#13645,#13646);
#11557=AXIS2_PLACEMENT_3D('',#17435,#13648,#13649);
#11558=AXIS2_PLACEMENT_3D('',#17439,#13652,#13653);
#11559=AXIS2_PLACEMENT_3D('',#17441,#13655,#13656);
#11560=AXIS2_PLACEMENT_3D('',#17443,#13658,#13659);
#11561=AXIS2_PLACEMENT_3D('',#17445,#13661,#13662);
#11562=AXIS2_PLACEMENT_3D('',#17447,#13664,#13665);
#11563=AXIS2_PLACEMENT_3D('',#17451,#13668,#13669);
#11564=AXIS2_PLACEMENT_3D('',#17455,#13672,#13673);
#11565=AXIS2_PLACEMENT_3D('',#17460,#13677,#13678);
#11566=AXIS2_PLACEMENT_3D('',#17462,#13680,#13681);
#11567=AXIS2_PLACEMENT_3D('',#17464,#13683,#13684);
#11568=AXIS2_PLACEMENT_3D('',#17466,#13686,#13687);
#11569=AXIS2_PLACEMENT_3D('',#17470,#13690,#13691);
#11570=AXIS2_PLACEMENT_3D('',#17474,#13694,#13695);
#11571=AXIS2_PLACEMENT_3D('',#17478,#13698,#13699);
#11572=AXIS2_PLACEMENT_3D('',#17482,#13702,#13703);
#11573=AXIS2_PLACEMENT_3D('',#17484,#13705,#13706);
#11574=AXIS2_PLACEMENT_3D('',#17486,#13708,#13709);
#11575=AXIS2_PLACEMENT_3D('',#17490,#13712,#13713);
#11576=AXIS2_PLACEMENT_3D('',#17495,#13717,#13718);
#11577=AXIS2_PLACEMENT_3D('',#17499,#13721,#13722);
#11578=AXIS2_PLACEMENT_3D('',#17505,#13726,#13727);
#11579=AXIS2_PLACEMENT_3D('',#17509,#13730,#13731);
#11580=AXIS2_PLACEMENT_3D('',#17513,#13734,#13735);
#11581=AXIS2_PLACEMENT_3D('',#17517,#13738,#13739);
#11582=AXIS2_PLACEMENT_3D('',#17521,#13742,#13743);
#11583=AXIS2_PLACEMENT_3D('',#17523,#13744,#13745);
#11584=AXIS2_PLACEMENT_3D('',#17529,#13749,#13750);
#11585=AXIS2_PLACEMENT_3D('',#17531,#13751,#13752);
#11586=AXIS2_PLACEMENT_3D('',#17533,#13754,#13755);
#11587=AXIS2_PLACEMENT_3D('',#17541,#13760,#13761);
#11588=AXIS2_PLACEMENT_3D('',#17544,#13764,#13765);
#11589=AXIS2_PLACEMENT_3D('',#17545,#13766,#13767);
#11590=AXIS2_PLACEMENT_3D('',#17549,#13770,#13771);
#11591=AXIS2_PLACEMENT_3D('',#17557,#13776,#13777);
#11592=AXIS2_PLACEMENT_3D('',#17565,#13782,#13783);
#11593=AXIS2_PLACEMENT_3D('',#17571,#13787,#13788);
#11594=AXIS2_PLACEMENT_3D('',#17579,#13793,#13794);
#11595=AXIS2_PLACEMENT_3D('',#17587,#13799,#13800);
#11596=AXIS2_PLACEMENT_3D('',#17593,#13804,#13805);
#11597=AXIS2_PLACEMENT_3D('',#17595,#13807,#13808);
#11598=AXIS2_PLACEMENT_3D('',#17597,#13810,#13811);
#11599=AXIS2_PLACEMENT_3D('',#17599,#13813,#13814);
#11600=AXIS2_PLACEMENT_3D('',#17603,#13817,#13818);
#11601=AXIS2_PLACEMENT_3D('',#17609,#13822,#13823);
#11602=AXIS2_PLACEMENT_3D('',#17613,#13826,#13827);
#11603=AXIS2_PLACEMENT_3D('',#17617,#13830,#13831);
#11604=AXIS2_PLACEMENT_3D('',#17621,#13834,#13835);
#11605=AXIS2_PLACEMENT_3D('',#17623,#13837,#13838);
#11606=AXIS2_PLACEMENT_3D('',#17625,#13840,#13841);
#11607=AXIS2_PLACEMENT_3D('',#17627,#13843,#13844);
#11608=AXIS2_PLACEMENT_3D('',#17628,#13845,#13846);
#11609=AXIS2_PLACEMENT_3D('',#17630,#13848,#13849);
#11610=AXIS2_PLACEMENT_3D('',#17632,#13851,#13852);
#11611=AXIS2_PLACEMENT_3D('',#17636,#13855,#13856);
#11612=AXIS2_PLACEMENT_3D('',#17649,#13865,#13866);
#11613=AXIS2_PLACEMENT_3D('',#17654,#13870,#13871);
#11614=AXIS2_PLACEMENT_3D('',#17655,#13872,#13873);
#11615=AXIS2_PLACEMENT_3D('',#17657,#13875,#13876);
#11616=AXIS2_PLACEMENT_3D('',#17667,#13882,#13883);
#11617=AXIS2_PLACEMENT_3D('',#17668,#13884,#13885);
#11618=AXIS2_PLACEMENT_3D('',#17670,#13887,#13888);
#11619=AXIS2_PLACEMENT_3D('',#17671,#13889,#13890);
#11620=AXIS2_PLACEMENT_3D('',#17673,#13892,#13893);
#11621=AXIS2_PLACEMENT_3D('',#17674,#13894,#13895);
#11622=AXIS2_PLACEMENT_3D('',#17675,#13896,#13897);
#11623=AXIS2_PLACEMENT_3D('',#17677,#13899,#13900);
#11624=AXIS2_PLACEMENT_3D('',#17678,#13901,#13902);
#11625=AXIS2_PLACEMENT_3D('',#17680,#13904,#13905);
#11626=AXIS2_PLACEMENT_3D('',#17684,#13908,#13909);
#11627=AXIS2_PLACEMENT_3D('',#17687,#13912,#13913);
#11628=AXIS2_PLACEMENT_3D('',#17689,#13915,#13916);
#11629=AXIS2_PLACEMENT_3D('',#17690,#13917,#13918);
#11630=AXIS2_PLACEMENT_3D('',#17692,#13920,#13921);
#11631=AXIS2_PLACEMENT_3D('',#17693,#13922,#13923);
#11632=AXIS2_PLACEMENT_3D('',#17696,#13926,#13927);
#11633=AXIS2_PLACEMENT_3D('',#17698,#13929,#13930);
#11634=AXIS2_PLACEMENT_3D('',#17699,#13931,#13932);
#11635=AXIS2_PLACEMENT_3D('',#17700,#13933,#13934);
#11636=AXIS2_PLACEMENT_3D('',#17755,#13935,#13936);
#11637=AXIS2_PLACEMENT_3D('',#17937,#13937,#13938);
#11638=AXIS2_PLACEMENT_3D('',#18119,#13939,#13940);
#11639=AXIS2_PLACEMENT_3D('',#18174,#13941,#13942);
#11640=AXIS2_PLACEMENT_3D('',#18229,#13943,#13944);
#11641=AXIS2_PLACEMENT_3D('',#18411,#13945,#13946);
#11642=AXIS2_PLACEMENT_3D('',#18412,#13947,#13948);
#11643=AXIS2_PLACEMENT_3D('',#18414,#13950,#13951);
#11644=AXIS2_PLACEMENT_3D('',#18415,#13952,#13953);
#11645=AXIS2_PLACEMENT_3D('',#18417,#13955,#13956);
#11646=AXIS2_PLACEMENT_3D('',#18418,#13957,#13958);
#11647=AXIS2_PLACEMENT_3D('',#18428,#13964,#13965);
#11648=AXIS2_PLACEMENT_3D('',#18429,#13966,#13967);
#11649=AXIS2_PLACEMENT_3D('',#18431,#13969,#13970);
#11650=AXIS2_PLACEMENT_3D('',#18435,#13973,#13974);
#11651=AXIS2_PLACEMENT_3D('',#18438,#13977,#13978);
#11652=AXIS2_PLACEMENT_3D('',#18441,#13981,#13982);
#11653=AXIS2_PLACEMENT_3D('',#18442,#13983,#13984);
#11654=AXIS2_PLACEMENT_3D('',#18443,#13985,#13986);
#11655=AXIS2_PLACEMENT_3D('',#18444,#13987,#13988);
#11656=AXIS2_PLACEMENT_3D('',#18445,#13989,#13990);
#11657=AXIS2_PLACEMENT_3D('',#18446,#13991,#13992);
#11658=AXIS2_PLACEMENT_3D('',#18447,#13993,#13994);
#11659=AXIS2_PLACEMENT_3D('',#18453,#13998,#13999);
#11660=AXIS2_PLACEMENT_3D('',#18457,#14002,#14003);
#11661=AXIS2_PLACEMENT_3D('',#18461,#14006,#14007);
#11662=AXIS2_PLACEMENT_3D('',#18727,#14009,#14010);
#11663=AXIS2_PLACEMENT_3D('',#18733,#14014,#14015);
#11664=AXIS2_PLACEMENT_3D('',#18737,#14018,#14019);
#11665=AXIS2_PLACEMENT_3D('',#18741,#14022,#14023);
#11666=AXIS2_PLACEMENT_3D('',#18743,#14025,#14026);
#11667=AXIS2_PLACEMENT_3D('',#18744,#14027,#14028);
#11668=AXIS2_PLACEMENT_3D('',#18745,#14029,#14030);
#11669=AXIS2_PLACEMENT_3D('',#18746,#14031,#14032);
#11670=AXIS2_PLACEMENT_3D('',#18747,#14033,#14034);
#11671=AXIS2_PLACEMENT_3D('',#18748,#14035,#14036);
#11672=AXIS2_PLACEMENT_3D('',#18749,#14037,#14038);
#11673=AXIS2_PLACEMENT_3D('',#18750,#14039,#14040);
#11674=AXIS2_PLACEMENT_3D('',#18751,#14041,#14042);
#11675=AXIS2_PLACEMENT_3D('',#18752,#14043,#14044);
#11676=AXIS2_PLACEMENT_3D('',#18754,#14045,#14046);
#11677=AXIS2_PLACEMENT_3D('',#18757,#14048,#14049);
#11678=AXIS2_PLACEMENT_3D('',#18758,#14050,#14051);
#11679=AXIS2_PLACEMENT_3D('',#18760,#14052,#14053);
#11680=AXIS2_PLACEMENT_3D('',#18763,#14055,#14056);
#11681=AXIS2_PLACEMENT_3D('',#18764,#14057,#14058);
#11682=AXIS2_PLACEMENT_3D('',#18766,#14059,#14060);
#11683=AXIS2_PLACEMENT_3D('',#18769,#14062,#14063);
#11684=AXIS2_PLACEMENT_3D('',#18770,#14064,#14065);
#11685=AXIS2_PLACEMENT_3D('',#18772,#14066,#14067);
#11686=AXIS2_PLACEMENT_3D('',#18775,#14069,#14070);
#11687=AXIS2_PLACEMENT_3D('',#18776,#14071,#14072);
#11688=AXIS2_PLACEMENT_3D('',#18778,#14073,#14074);
#11689=AXIS2_PLACEMENT_3D('',#18781,#14076,#14077);
#11690=AXIS2_PLACEMENT_3D('',#18782,#14078,#14079);
#11691=AXIS2_PLACEMENT_3D('',#18784,#14080,#14081);
#11692=AXIS2_PLACEMENT_3D('',#18787,#14083,#14084);
#11693=AXIS2_PLACEMENT_3D('',#18788,#14085,#14086);
#11694=AXIS2_PLACEMENT_3D('',#18790,#14087,#14088);
#11695=AXIS2_PLACEMENT_3D('',#18793,#14090,#14091);
#11696=AXIS2_PLACEMENT_3D('',#18794,#14092,#14093);
#11697=AXIS2_PLACEMENT_3D('',#18796,#14094,#14095);
#11698=AXIS2_PLACEMENT_3D('',#18799,#14097,#14098);
#11699=AXIS2_PLACEMENT_3D('',#18800,#14099,#14100);
#11700=AXIS2_PLACEMENT_3D('',#18802,#14101,#14102);
#11701=AXIS2_PLACEMENT_3D('',#18805,#14104,#14105);
#11702=AXIS2_PLACEMENT_3D('',#18806,#14106,#14107);
#11703=AXIS2_PLACEMENT_3D('',#18808,#14108,#14109);
#11704=AXIS2_PLACEMENT_3D('',#18811,#14111,#14112);
#11705=AXIS2_PLACEMENT_3D('',#18812,#14113,#14114);
#11706=AXIS2_PLACEMENT_3D('',#18814,#14115,#14116);
#11707=AXIS2_PLACEMENT_3D('',#18817,#14118,#14119);
#11708=AXIS2_PLACEMENT_3D('',#18818,#14120,#14121);
#11709=AXIS2_PLACEMENT_3D('',#18820,#14122,#14123);
#11710=AXIS2_PLACEMENT_3D('',#18823,#14125,#14126);
#11711=AXIS2_PLACEMENT_3D('',#18824,#14127,#14128);
#11712=AXIS2_PLACEMENT_3D('',#18826,#14129,#14130);
#11713=AXIS2_PLACEMENT_3D('',#18829,#14132,#14133);
#11714=AXIS2_PLACEMENT_3D('',#18830,#14134,#14135);
#11715=AXIS2_PLACEMENT_3D('',#18832,#14136,#14137);
#11716=AXIS2_PLACEMENT_3D('',#18835,#14139,#14140);
#11717=AXIS2_PLACEMENT_3D('',#18836,#14141,#14142);
#11718=AXIS2_PLACEMENT_3D('',#18838,#14143,#14144);
#11719=AXIS2_PLACEMENT_3D('',#18841,#14146,#14147);
#11720=AXIS2_PLACEMENT_3D('',#18842,#14148,#14149);
#11721=AXIS2_PLACEMENT_3D('',#18844,#14150,#14151);
#11722=AXIS2_PLACEMENT_3D('',#18847,#14153,#14154);
#11723=AXIS2_PLACEMENT_3D('',#18848,#14155,#14156);
#11724=AXIS2_PLACEMENT_3D('',#18850,#14157,#14158);
#11725=AXIS2_PLACEMENT_3D('',#18853,#14160,#14161);
#11726=AXIS2_PLACEMENT_3D('',#18854,#14162,#14163);
#11727=AXIS2_PLACEMENT_3D('',#18856,#14164,#14165);
#11728=AXIS2_PLACEMENT_3D('',#18859,#14167,#14168);
#11729=AXIS2_PLACEMENT_3D('',#18860,#14169,#14170);
#11730=AXIS2_PLACEMENT_3D('',#18862,#14171,#14172);
#11731=AXIS2_PLACEMENT_3D('',#18865,#14174,#14175);
#11732=AXIS2_PLACEMENT_3D('',#18866,#14176,#14177);
#11733=AXIS2_PLACEMENT_3D('',#18868,#14178,#14179);
#11734=AXIS2_PLACEMENT_3D('',#18871,#14181,#14182);
#11735=AXIS2_PLACEMENT_3D('',#18872,#14183,#14184);
#11736=AXIS2_PLACEMENT_3D('',#18874,#14185,#14186);
#11737=AXIS2_PLACEMENT_3D('',#18877,#14188,#14189);
#11738=AXIS2_PLACEMENT_3D('',#18878,#14190,#14191);
#11739=AXIS2_PLACEMENT_3D('',#18880,#14192,#14193);
#11740=AXIS2_PLACEMENT_3D('',#18883,#14195,#14196);
#11741=AXIS2_PLACEMENT_3D('',#18884,#14197,#14198);
#11742=AXIS2_PLACEMENT_3D('',#18886,#14199,#14200);
#11743=AXIS2_PLACEMENT_3D('',#18889,#14202,#14203);
#11744=AXIS2_PLACEMENT_3D('',#18890,#14204,#14205);
#11745=AXIS2_PLACEMENT_3D('',#18892,#14206,#14207);
#11746=AXIS2_PLACEMENT_3D('',#18895,#14209,#14210);
#11747=AXIS2_PLACEMENT_3D('',#18896,#14211,#14212);
#11748=AXIS2_PLACEMENT_3D('',#18898,#14213,#14214);
#11749=AXIS2_PLACEMENT_3D('',#18901,#14216,#14217);
#11750=AXIS2_PLACEMENT_3D('',#18902,#14218,#14219);
#11751=AXIS2_PLACEMENT_3D('',#18905,#14221,#14222);
#11752=AXIS2_PLACEMENT_3D('',#18906,#14223,#14224);
#11753=AXIS2_PLACEMENT_3D('',#18909,#14226,#14227);
#11754=AXIS2_PLACEMENT_3D('',#18910,#14228,#14229);
#11755=AXIS2_PLACEMENT_3D('',#18913,#14231,#14232);
#11756=AXIS2_PLACEMENT_3D('',#18914,#14233,#14234);
#11757=AXIS2_PLACEMENT_3D('',#18917,#14236,#14237);
#11758=AXIS2_PLACEMENT_3D('',#18918,#14238,#14239);
#11759=AXIS2_PLACEMENT_3D('',#18921,#14241,#14242);
#11760=AXIS2_PLACEMENT_3D('',#18922,#14243,#14244);
#11761=AXIS2_PLACEMENT_3D('',#18925,#14246,#14247);
#11762=AXIS2_PLACEMENT_3D('',#18926,#14248,#14249);
#11763=AXIS2_PLACEMENT_3D('',#18929,#14251,#14252);
#11764=AXIS2_PLACEMENT_3D('',#18930,#14253,#14254);
#11765=AXIS2_PLACEMENT_3D('',#18933,#14256,#14257);
#11766=AXIS2_PLACEMENT_3D('',#18934,#14258,#14259);
#11767=AXIS2_PLACEMENT_3D('',#18937,#14261,#14262);
#11768=AXIS2_PLACEMENT_3D('',#18938,#14263,#14264);
#11769=AXIS2_PLACEMENT_3D('',#18940,#14265,#14266);
#11770=AXIS2_PLACEMENT_3D('',#18943,#14268,#14269);
#11771=AXIS2_PLACEMENT_3D('',#18944,#14270,#14271);
#11772=AXIS2_PLACEMENT_3D('',#18946,#14272,#14273);
#11773=AXIS2_PLACEMENT_3D('',#18949,#14275,#14276);
#11774=AXIS2_PLACEMENT_3D('',#18950,#14277,#14278);
#11775=AXIS2_PLACEMENT_3D('',#18952,#14279,#14280);
#11776=AXIS2_PLACEMENT_3D('',#18955,#14282,#14283);
#11777=AXIS2_PLACEMENT_3D('',#18956,#14284,#14285);
#11778=AXIS2_PLACEMENT_3D('',#18958,#14286,#14287);
#11779=AXIS2_PLACEMENT_3D('',#18961,#14289,#14290);
#11780=AXIS2_PLACEMENT_3D('',#18962,#14291,#14292);
#11781=AXIS2_PLACEMENT_3D('',#18964,#14293,#14294);
#11782=AXIS2_PLACEMENT_3D('',#18967,#14296,#14297);
#11783=AXIS2_PLACEMENT_3D('',#18968,#14298,#14299);
#11784=AXIS2_PLACEMENT_3D('',#18970,#14300,#14301);
#11785=AXIS2_PLACEMENT_3D('',#18973,#14303,#14304);
#11786=AXIS2_PLACEMENT_3D('',#18974,#14305,#14306);
#11787=AXIS2_PLACEMENT_3D('',#18976,#14307,#14308);
#11788=AXIS2_PLACEMENT_3D('',#18979,#14310,#14311);
#11789=AXIS2_PLACEMENT_3D('',#18980,#14312,#14313);
#11790=AXIS2_PLACEMENT_3D('',#18982,#14314,#14315);
#11791=AXIS2_PLACEMENT_3D('',#18985,#14317,#14318);
#11792=AXIS2_PLACEMENT_3D('',#18986,#14319,#14320);
#11793=AXIS2_PLACEMENT_3D('',#18993,#14323,#14324);
#11794=AXIS2_PLACEMENT_3D('',#18997,#14326,#14327);
#11795=AXIS2_PLACEMENT_3D('',#18999,#14329,#14330);
#11796=AXIS2_PLACEMENT_3D('',#19001,#14331,#14332);
#11797=AXIS2_PLACEMENT_3D('',#19018,#14333,#14334);
#11798=AXIS2_PLACEMENT_3D('',#19020,#14336,#14337);
#11799=AXIS2_PLACEMENT_3D('',#19028,#14341,#14342);
#11800=AXIS2_PLACEMENT_3D('',#19032,#14344,#14345);
#11801=AXIS2_PLACEMENT_3D('',#19039,#14349,#14350);
#11802=AXIS2_PLACEMENT_3D('',#19040,#14351,#14352);
#11803=AXIS2_PLACEMENT_3D('',#19044,#14354,#14355);
#11804=AXIS2_PLACEMENT_3D('',#19059,#14356,#14357);
#11805=AXIS2_PLACEMENT_3D('',#19065,#14360,#14361);
#11806=AXIS2_PLACEMENT_3D('',#19067,#14363,#14364);
#11807=AXIS2_PLACEMENT_3D('',#19071,#14367,#14368);
#11808=AXIS2_PLACEMENT_3D('',#19073,#14369,#14370);
#11809=AXIS2_PLACEMENT_3D('',#19077,#14373,#14374);
#11810=AXIS2_PLACEMENT_3D('',#19080,#14377,#14378);
#11811=AXIS2_PLACEMENT_3D('',#19084,#14380,#14381);
#11812=AXIS2_PLACEMENT_3D('',#19088,#14383,#14384);
#11813=AXIS2_PLACEMENT_3D('',#19091,#14386,#14387);
#11814=AXIS2_PLACEMENT_3D('',#19196,#14390,#14391);
#11815=AXIS2_PLACEMENT_3D('',#19199,#14392,#14393);
#11816=AXIS2_PLACEMENT_3D('',#19203,#14395,#14396);
#11817=AXIS2_PLACEMENT_3D('',#19206,#14398,#14399);
#11818=AXIS2_PLACEMENT_3D('',#19208,#14401,#14402);
#11819=AXIS2_PLACEMENT_3D('',#19211,#14404,#14405);
#11820=AXIS2_PLACEMENT_3D('',#19212,#14406,#14407);
#11821=AXIS2_PLACEMENT_3D('',#19214,#14408,#14409);
#11822=AXIS2_PLACEMENT_3D('',#19216,#14411,#14412);
#11823=AXIS2_PLACEMENT_3D('',#19223,#14417,#14418);
#11824=AXIS2_PLACEMENT_3D('',#19225,#14419,#14420);
#11825=AXIS2_PLACEMENT_3D('',#19227,#14422,#14423);
#11826=AXIS2_PLACEMENT_3D('',#19231,#14425,#14426);
#11827=AXIS2_PLACEMENT_3D('',#19233,#14428,#14429);
#11828=AXIS2_PLACEMENT_3D('',#19237,#14432,#14433);
#11829=AXIS2_PLACEMENT_3D('',#19238,#14434,#14435);
#11830=AXIS2_PLACEMENT_3D('',#19290,#14438,#14439);
#11831=AXIS2_PLACEMENT_3D('',#19296,#14443,#14444);
#11832=AXIS2_PLACEMENT_3D('',#19298,#14445,#14446);
#11833=AXIS2_PLACEMENT_3D('',#19300,#14448,#14449);
#11834=AXIS2_PLACEMENT_3D('',#19304,#14451,#14452);
#11835=AXIS2_PLACEMENT_3D('',#19306,#14454,#14455);
#11836=AXIS2_PLACEMENT_3D('',#19308,#14457,#14458);
#11837=AXIS2_PLACEMENT_3D('',#19309,#14459,#14460);
#11838=AXIS2_PLACEMENT_3D('',#19310,#14461,#14462);
#11839=AXIS2_PLACEMENT_3D('',#19312,#14464,#14465);
#11840=AXIS2_PLACEMENT_3D('',#19314,#14467,#14468);
#11841=AXIS2_PLACEMENT_3D('',#19315,#14469,#14470);
#11842=AXIS2_PLACEMENT_3D('',#19316,#14471,#14472);
#11843=AXIS2_PLACEMENT_3D('',#19318,#14473,#14474);
#11844=AXIS2_PLACEMENT_3D('',#19321,#14476,#14477);
#11845=AXIS2_PLACEMENT_3D('',#19322,#14478,#14479);
#11846=AXIS2_PLACEMENT_3D('',#19324,#14480,#14481);
#11847=AXIS2_PLACEMENT_3D('',#19327,#14483,#14484);
#11848=AXIS2_PLACEMENT_3D('',#19328,#14485,#14486);
#11849=AXIS2_PLACEMENT_3D('',#19330,#14487,#14488);
#11850=AXIS2_PLACEMENT_3D('',#19333,#14490,#14491);
#11851=AXIS2_PLACEMENT_3D('',#19334,#14492,#14493);
#11852=AXIS2_PLACEMENT_3D('',#19336,#14494,#14495);
#11853=AXIS2_PLACEMENT_3D('',#19339,#14497,#14498);
#11854=AXIS2_PLACEMENT_3D('',#19340,#14499,#14500);
#11855=AXIS2_PLACEMENT_3D('',#19342,#14501,#14502);
#11856=AXIS2_PLACEMENT_3D('',#19345,#14504,#14505);
#11857=AXIS2_PLACEMENT_3D('',#19346,#14506,#14507);
#11858=AXIS2_PLACEMENT_3D('',#19348,#14508,#14509);
#11859=AXIS2_PLACEMENT_3D('',#19351,#14511,#14512);
#11860=AXIS2_PLACEMENT_3D('',#19352,#14513,#14514);
#11861=AXIS2_PLACEMENT_3D('',#19354,#14515,#14516);
#11862=AXIS2_PLACEMENT_3D('',#19357,#14518,#14519);
#11863=AXIS2_PLACEMENT_3D('',#19358,#14520,#14521);
#11864=AXIS2_PLACEMENT_3D('',#19360,#14522,#14523);
#11865=AXIS2_PLACEMENT_3D('',#19363,#14525,#14526);
#11866=AXIS2_PLACEMENT_3D('',#19364,#14527,#14528);
#11867=AXIS2_PLACEMENT_3D('',#19365,#14529,#14530);
#11868=AXIS2_PLACEMENT_3D('',#19368,#14531,#14532);
#11869=AXIS2_PLACEMENT_3D('',#19371,#14534,#14535);
#11870=AXIS2_PLACEMENT_3D('',#19372,#14536,#14537);
#11871=AXIS2_PLACEMENT_3D('',#19373,#14538,#14539);
#11872=AXIS2_PLACEMENT_3D('',#19375,#14540,#14541);
#11873=AXIS2_PLACEMENT_3D('',#19378,#14543,#14544);
#11874=AXIS2_PLACEMENT_3D('',#19379,#14545,#14546);
#11875=AXIS2_PLACEMENT_3D('',#19381,#14547,#14548);
#11876=AXIS2_PLACEMENT_3D('',#19384,#14550,#14551);
#11877=AXIS2_PLACEMENT_3D('',#19385,#14552,#14553);
#11878=AXIS2_PLACEMENT_3D('',#19387,#14554,#14555);
#11879=AXIS2_PLACEMENT_3D('',#19390,#14557,#14558);
#11880=AXIS2_PLACEMENT_3D('',#19391,#14559,#14560);
#11881=AXIS2_PLACEMENT_3D('',#19393,#14561,#14562);
#11882=AXIS2_PLACEMENT_3D('',#19396,#14564,#14565);
#11883=AXIS2_PLACEMENT_3D('',#19397,#14566,#14567);
#11884=AXIS2_PLACEMENT_3D('',#19399,#14568,#14569);
#11885=AXIS2_PLACEMENT_3D('',#19402,#14571,#14572);
#11886=AXIS2_PLACEMENT_3D('',#19403,#14573,#14574);
#11887=AXIS2_PLACEMENT_3D('',#19405,#14575,#14576);
#11888=AXIS2_PLACEMENT_3D('',#19408,#14578,#14579);
#11889=AXIS2_PLACEMENT_3D('',#19409,#14580,#14581);
#11890=AXIS2_PLACEMENT_3D('',#19411,#14582,#14583);
#11891=AXIS2_PLACEMENT_3D('',#19414,#14585,#14586);
#11892=AXIS2_PLACEMENT_3D('',#19415,#14587,#14588);
#11893=AXIS2_PLACEMENT_3D('',#19417,#14589,#14590);
#11894=AXIS2_PLACEMENT_3D('',#19420,#14592,#14593);
#11895=AXIS2_PLACEMENT_3D('',#19421,#14594,#14595);
#11896=AXIS2_PLACEMENT_3D('',#19423,#14596,#14597);
#11897=AXIS2_PLACEMENT_3D('',#19426,#14599,#14600);
#11898=AXIS2_PLACEMENT_3D('',#19427,#14601,#14602);
#11899=AXIS2_PLACEMENT_3D('',#19430,#14604,#14605);
#11900=AXIS2_PLACEMENT_3D('',#19431,#14606,#14607);
#11901=AXIS2_PLACEMENT_3D('',#19436,#14609,#14610);
#11902=AXIS2_PLACEMENT_3D('',#19439,#14612,#14613);
#11903=AXIS2_PLACEMENT_3D('',#19440,#14614,#14615);
#11904=AXIS2_PLACEMENT_3D('',#19443,#14616,#14617);
#11905=AXIS2_PLACEMENT_3D('',#19447,#14619,#14620);
#11906=AXIS2_PLACEMENT_3D('',#19449,#14622,#14623);
#11907=AXIS2_PLACEMENT_3D('',#19452,#14626,#14627);
#11908=AXIS2_PLACEMENT_3D('',#19455,#14630,#14631);
#11909=AXIS2_PLACEMENT_3D('',#19456,#14632,#14633);
#11910=AXIS2_PLACEMENT_3D('',#19457,#14634,#14635);
#11911=AXIS2_PLACEMENT_3D('',#19458,#14636,#14637);
#11912=AXIS2_PLACEMENT_3D('',#19459,#14638,#14639);
#11913=AXIS2_PLACEMENT_3D('',#19461,#14640,#14641);
#11914=AXIS2_PLACEMENT_3D('',#19464,#14643,#14644);
#11915=AXIS2_PLACEMENT_3D('',#19465,#14645,#14646);
#11916=AXIS2_PLACEMENT_3D('',#19467,#14647,#14648);
#11917=AXIS2_PLACEMENT_3D('',#19470,#14650,#14651);
#11918=AXIS2_PLACEMENT_3D('',#19471,#14652,#14653);
#11919=AXIS2_PLACEMENT_3D('',#19473,#14654,#14655);
#11920=AXIS2_PLACEMENT_3D('',#19476,#14657,#14658);
#11921=AXIS2_PLACEMENT_3D('',#19477,#14659,#14660);
#11922=AXIS2_PLACEMENT_3D('',#19480,#14661,#14662);
#11923=AXIS2_PLACEMENT_3D('',#19484,#14664,#14665);
#11924=AXIS2_PLACEMENT_3D('',#19486,#14667,#14668);
#11925=AXIS2_PLACEMENT_3D('',#19488,#14669,#14670);
#11926=AXIS2_PLACEMENT_3D('',#19491,#14672,#14673);
#11927=AXIS2_PLACEMENT_3D('',#19492,#14674,#14675);
#11928=AXIS2_PLACEMENT_3D('',#19494,#14676,#14677);
#11929=AXIS2_PLACEMENT_3D('',#19497,#14679,#14680);
#11930=AXIS2_PLACEMENT_3D('',#19498,#14681,#14682);
#11931=AXIS2_PLACEMENT_3D('',#19519,#14693,#14694);
#11932=AXIS2_PLACEMENT_3D('',#19525,#14698,#14699);
#11933=AXIS2_PLACEMENT_3D('',#19531,#14703,#14704);
#11934=AXIS2_PLACEMENT_3D('',#19540,#14709,#14710);
#11935=AXIS2_PLACEMENT_3D('',#19546,#14714,#14715);
#11936=AXIS2_PLACEMENT_3D('',#19558,#14723,#14724);
#11937=AXIS2_PLACEMENT_3D('',#19567,#14729,#14730);
#11938=AXIS2_PLACEMENT_3D('',#19568,#14731,#14732);
#11939=AXIS2_PLACEMENT_3D('',#19569,#14733,#14734);
#11940=AXIS2_PLACEMENT_3D('',#19570,#14735,#14736);
#11941=AXIS2_PLACEMENT_3D('',#19571,#14737,#14738);
#11942=AXIS2_PLACEMENT_3D('',#19572,#14739,#14740);
#11943=AXIS2_PLACEMENT_3D('',#19573,#14741,#14742);
#11944=AXIS2_PLACEMENT_3D('',#19576,#14744,#14745);
#11945=AXIS2_PLACEMENT_3D('',#19578,#14747,#14748);
#11946=AXIS2_PLACEMENT_3D('',#19579,#14749,#14750);
#11947=AXIS2_PLACEMENT_3D('',#19582,#14752,#14753);
#11948=AXIS2_PLACEMENT_3D('',#19583,#14754,#14755);
#11949=AXIS2_PLACEMENT_3D('',#19585,#14757,#14758);
#11950=AXIS2_PLACEMENT_3D('',#19586,#14759,#14760);
#11951=AXIS2_PLACEMENT_3D('',#19587,#14761,#14762);
#11952=AXIS2_PLACEMENT_3D('',#19588,#14763,#14764);
#11953=AXIS2_PLACEMENT_3D('',#19589,#14765,#14766);
#11954=AXIS2_PLACEMENT_3D('',#19591,#14768,#14769);
#11955=AXIS2_PLACEMENT_3D('',#19592,#14770,#14771);
#11956=AXIS2_PLACEMENT_3D('',#19593,#14772,#14773);
#11957=AXIS2_PLACEMENT_3D('',#19594,#14774,#14775);
#11958=AXIS2_PLACEMENT_3D('',#19603,#14780,#14781);
#11959=AXIS2_PLACEMENT_3D('',#19609,#14785,#14786);
#11960=AXIS2_PLACEMENT_3D('',#19615,#14790,#14791);
#11961=AXIS2_PLACEMENT_3D('',#19618,#14794,#14795);
#11962=AXIS2_PLACEMENT_3D('',#19619,#14796,#14797);
#11963=AXIS2_PLACEMENT_3D('',#19620,#14798,#14799);
#11964=AXIS2_PLACEMENT_3D('',#19621,#14800,#14801);
#11965=AXIS2_PLACEMENT_3D('',#19622,#14802,#14803);
#11966=AXIS2_PLACEMENT_3D('',#19624,#14804,#14805);
#11967=AXIS2_PLACEMENT_3D('',#19627,#14807,#14808);
#11968=AXIS2_PLACEMENT_3D('',#19628,#14809,#14810);
#11969=AXIS2_PLACEMENT_3D('',#19630,#14811,#14812);
#11970=AXIS2_PLACEMENT_3D('',#19633,#14814,#14815);
#11971=AXIS2_PLACEMENT_3D('',#19634,#14816,#14817);
#11972=AXIS2_PLACEMENT_3D('',#19636,#14818,#14819);
#11973=AXIS2_PLACEMENT_3D('',#19639,#14821,#14822);
#11974=AXIS2_PLACEMENT_3D('',#19640,#14823,#14824);
#11975=AXIS2_PLACEMENT_3D('',#19642,#14825,#14826);
#11976=AXIS2_PLACEMENT_3D('',#19645,#14828,#14829);
#11977=AXIS2_PLACEMENT_3D('',#19646,#14830,#14831);
#11978=AXIS2_PLACEMENT_3D('',#19648,#14832,#14833);
#11979=AXIS2_PLACEMENT_3D('',#19651,#14835,#14836);
#11980=AXIS2_PLACEMENT_3D('',#19652,#14837,#14838);
#11981=AXIS2_PLACEMENT_3D('',#19661,#14843,#14844);
#11982=AXIS2_PLACEMENT_3D('',#19671,#14850,#14851);
#11983=AXIS2_PLACEMENT_3D('',#19677,#14855,#14856);
#11984=AXIS2_PLACEMENT_3D('',#19687,#14862,#14863);
#11985=AXIS2_PLACEMENT_3D('',#19693,#14867,#14868);
#11986=AXIS2_PLACEMENT_3D('',#19703,#14874,#14875);
#11987=AXIS2_PLACEMENT_3D('',#19713,#14881,#14882);
#11988=AXIS2_PLACEMENT_3D('',#19725,#14890,#14891);
#11989=AXIS2_PLACEMENT_3D('',#19737,#14899,#14900);
#11990=AXIS2_PLACEMENT_3D('',#19738,#14901,#14902);
#11991=AXIS2_PLACEMENT_3D('',#19739,#14903,#14904);
#11992=AXIS2_PLACEMENT_3D('',#19740,#14905,#14906);
#11993=AXIS2_PLACEMENT_3D('',#19741,#14907,#14908);
#11994=AXIS2_PLACEMENT_3D('',#19744,#14909,#14910);
#11995=AXIS2_PLACEMENT_3D('',#19748,#14912,#14913);
#11996=AXIS2_PLACEMENT_3D('',#19750,#14915,#14916);
#11997=AXIS2_PLACEMENT_3D('',#19756,#14920,#14921);
#11998=AXIS2_PLACEMENT_3D('',#19762,#14925,#14926);
#11999=AXIS2_PLACEMENT_3D('',#19763,#14927,#14928);
#12000=AXIS2_PLACEMENT_3D('',#19764,#14929,#14930);
#12001=AXIS2_PLACEMENT_3D('',#19765,#14931,#14932);
#12002=AXIS2_PLACEMENT_3D('',#19766,#14933,#14934);
#12003=AXIS2_PLACEMENT_3D('',#19767,#14935,#14936);
#12004=AXIS2_PLACEMENT_3D('',#19768,#14937,#14938);
#12005=AXIS2_PLACEMENT_3D('',#19770,#14940,#14941);
#12006=AXIS2_PLACEMENT_3D('',#19772,#14943,#14944);
#12007=AXIS2_PLACEMENT_3D('',#19774,#14946,#14947);
#12008=AXIS2_PLACEMENT_3D('',#19776,#14949,#14950);
#12009=AXIS2_PLACEMENT_3D('',#19777,#14951,#14952);
#12010=AXIS2_PLACEMENT_3D('',#19778,#14953,#14954);
#12011=AXIS2_PLACEMENT_3D('',#19779,#14955,#14956);
#12012=AXIS2_PLACEMENT_3D('',#19781,#14957,#14958);
#12013=AXIS2_PLACEMENT_3D('',#19783,#14959,#14960);
#12014=AXIS2_PLACEMENT_3D('',#19784,#14961,#14962);
#12015=AXIS2_PLACEMENT_3D('',#19785,#14963,#14964);
#12016=AXIS2_PLACEMENT_3D('',#19787,#14965,#14966);
#12017=AXIS2_PLACEMENT_3D('',#19790,#14968,#14969);
#12018=AXIS2_PLACEMENT_3D('',#19791,#14970,#14971);
#12019=AXIS2_PLACEMENT_3D('',#19794,#14972,#14973);
#12020=AXIS2_PLACEMENT_3D('',#19795,#14974,#14975);
#12021=AXIS2_PLACEMENT_3D('',#19797,#14977,#14978);
#12022=AXIS2_PLACEMENT_3D('',#19800,#14980,#14981);
#12023=AXIS2_PLACEMENT_3D('',#19801,#14982,#14983);
#12024=AXIS2_PLACEMENT_3D('',#19804,#14985,#14986);
#12025=AXIS2_PLACEMENT_3D('',#19805,#14987,#14988);
#12026=AXIS2_PLACEMENT_3D('',#19807,#14989,#14990);
#12027=AXIS2_PLACEMENT_3D('',#19809,#14992,#14993);
#12028=AXIS2_PLACEMENT_3D('',#19810,#14994,#14995);
#12029=AXIS2_PLACEMENT_3D('',#19811,#14996,#14997);
#12030=AXIS2_PLACEMENT_3D('',#19814,#14998,#14999);
#12031=AXIS2_PLACEMENT_3D('',#19815,#15000,#15001);
#12032=AXIS2_PLACEMENT_3D('',#19818,#15002,#15003);
#12033=AXIS2_PLACEMENT_3D('',#19819,#15004,#15005);
#12034=AXIS2_PLACEMENT_3D('',#19822,#15006,#15007);
#12035=AXIS2_PLACEMENT_3D('',#19823,#15008,#15009);
#12036=AXIS2_PLACEMENT_3D('',#19826,#15010,#15011);
#12037=AXIS2_PLACEMENT_3D('',#19827,#15012,#15013);
#12038=AXIS2_PLACEMENT_3D('',#19830,#15014,#15015);
#12039=AXIS2_PLACEMENT_3D('',#19831,#15016,#15017);
#12040=AXIS2_PLACEMENT_3D('',#19834,#15018,#15019);
#12041=AXIS2_PLACEMENT_3D('',#19835,#15020,#15021);
#12042=AXIS2_PLACEMENT_3D('',#19838,#15022,#15023);
#12043=AXIS2_PLACEMENT_3D('',#19839,#15024,#15025);
#12044=AXIS2_PLACEMENT_3D('',#19842,#15026,#15027);
#12045=AXIS2_PLACEMENT_3D('',#19843,#15028,#15029);
#12046=AXIS2_PLACEMENT_3D('',#19846,#15030,#15031);
#12047=AXIS2_PLACEMENT_3D('',#19847,#15032,#15033);
#12048=AXIS2_PLACEMENT_3D('',#19850,#15034,#15035);
#12049=AXIS2_PLACEMENT_3D('',#19851,#15036,#15037);
#12050=AXIS2_PLACEMENT_3D('',#19854,#15038,#15039);
#12051=AXIS2_PLACEMENT_3D('',#19855,#15040,#15041);
#12052=AXIS2_PLACEMENT_3D('',#19858,#15042,#15043);
#12053=AXIS2_PLACEMENT_3D('',#19859,#15044,#15045);
#12054=AXIS2_PLACEMENT_3D('',#19861,#15046,#15047);
#12055=AXIS2_PLACEMENT_3D('',#19864,#15049,#15050);
#12056=AXIS2_PLACEMENT_3D('',#19865,#15051,#15052);
#12057=AXIS2_PLACEMENT_3D('',#19867,#15053,#15054);
#12058=AXIS2_PLACEMENT_3D('',#19870,#15056,#15057);
#12059=AXIS2_PLACEMENT_3D('',#19871,#15058,#15059);
#12060=AXIS2_PLACEMENT_3D('',#19872,#15060,#15061);
#12061=AXIS2_PLACEMENT_3D('',#19873,#15062,#15063);
#12062=AXIS2_PLACEMENT_3D('',#19875,#15064,#15065);
#12063=AXIS2_PLACEMENT_3D('',#19878,#15067,#15068);
#12064=AXIS2_PLACEMENT_3D('',#19879,#15069,#15070);
#12065=AXIS2_PLACEMENT_3D('',#19881,#15071,#15072);
#12066=AXIS2_PLACEMENT_3D('',#19884,#15074,#15075);
#12067=AXIS2_PLACEMENT_3D('',#19885,#15076,#15077);
#12068=AXIS2_PLACEMENT_3D('',#19886,#15078,#15079);
#12069=AXIS2_PLACEMENT_3D('',#19887,#15080,#15081);
#12070=AXIS2_PLACEMENT_3D('',#19889,#15082,#15083);
#12071=AXIS2_PLACEMENT_3D('',#19892,#15085,#15086);
#12072=AXIS2_PLACEMENT_3D('',#19893,#15087,#15088);
#12073=AXIS2_PLACEMENT_3D('',#19895,#15089,#15090);
#12074=AXIS2_PLACEMENT_3D('',#19898,#15092,#15093);
#12075=AXIS2_PLACEMENT_3D('',#19899,#15094,#15095);
#12076=AXIS2_PLACEMENT_3D('',#19901,#15096,#15097);
#12077=AXIS2_PLACEMENT_3D('',#19902,#15098,#15099);
#12078=AXIS2_PLACEMENT_3D('',#19903,#15100,#15101);
#12079=AXIS2_PLACEMENT_3D('',#19905,#15102,#15103);
#12080=AXIS2_PLACEMENT_3D('',#19907,#15105,#15106);
#12081=AXIS2_PLACEMENT_3D('',#19910,#15107,#15108);
#12082=AXIS2_PLACEMENT_3D('',#19911,#15109,#15110);
#12083=AXIS2_PLACEMENT_3D('',#19914,#15112,#15113);
#12084=AXIS2_PLACEMENT_3D('',#19915,#15114,#15115);
#12085=AXIS2_PLACEMENT_3D('',#19918,#15117,#15118);
#12086=AXIS2_PLACEMENT_3D('',#19919,#15119,#15120);
#12087=AXIS2_PLACEMENT_3D('',#19920,#15121,#15122);
#12088=AXIS2_PLACEMENT_3D('',#19921,#15123,#15124);
#12089=AXIS2_PLACEMENT_3D('',#19922,#15125,#15126);
#12090=AXIS2_PLACEMENT_3D('',#19923,#15127,#15128);
#12091=AXIS2_PLACEMENT_3D('',#19925,#15129,#15130);
#12092=AXIS2_PLACEMENT_3D('',#19928,#15132,#15133);
#12093=AXIS2_PLACEMENT_3D('',#19929,#15134,#15135);
#12094=AXIS2_PLACEMENT_3D('',#19931,#15136,#15137);
#12095=AXIS2_PLACEMENT_3D('',#19934,#15139,#15140);
#12096=AXIS2_PLACEMENT_3D('',#19935,#15141,#15142);
#12097=AXIS2_PLACEMENT_3D('',#19937,#15143,#15144);
#12098=AXIS2_PLACEMENT_3D('',#19940,#15146,#15147);
#12099=AXIS2_PLACEMENT_3D('',#19941,#15148,#15149);
#12100=AXIS2_PLACEMENT_3D('',#19942,#15150,#15151);
#12101=AXIS2_PLACEMENT_3D('',#19943,#15152,#15153);
#12102=AXIS2_PLACEMENT_3D('',#19944,#15154,#15155);
#12103=AXIS2_PLACEMENT_3D('',#19945,#15156,#15157);
#12104=AXIS2_PLACEMENT_3D('',#19947,#15158,#15159);
#12105=AXIS2_PLACEMENT_3D('',#19950,#15161,#15162);
#12106=AXIS2_PLACEMENT_3D('',#19951,#15163,#15164);
#12107=AXIS2_PLACEMENT_3D('',#19953,#15165,#15166);
#12108=AXIS2_PLACEMENT_3D('',#19956,#15168,#15169);
#12109=AXIS2_PLACEMENT_3D('',#19957,#15170,#15171);
#12110=AXIS2_PLACEMENT_3D('',#19959,#15172,#15173);
#12111=AXIS2_PLACEMENT_3D('',#19962,#15175,#15176);
#12112=AXIS2_PLACEMENT_3D('',#19963,#15177,#15178);
#12113=AXIS2_PLACEMENT_3D('',#19964,#15179,#15180);
#12114=AXIS2_PLACEMENT_3D('',#19965,#15181,#15182);
#12115=AXIS2_PLACEMENT_3D('',#19966,#15183,#15184);
#12116=AXIS2_PLACEMENT_3D('',#19967,#15185,#15186);
#12117=AXIS2_PLACEMENT_3D('',#19968,#15187,#15188);
#12118=AXIS2_PLACEMENT_3D('',#19969,#15189,#15190);
#12119=AXIS2_PLACEMENT_3D('',#19970,#15191,#15192);
#12120=AXIS2_PLACEMENT_3D('',#19971,#15193,#15194);
#12121=AXIS2_PLACEMENT_3D('',#19972,#15195,#15196);
#12122=AXIS2_PLACEMENT_3D('',#19973,#15197,#15198);
#12123=AXIS2_PLACEMENT_3D('',#19974,#15199,#15200);
#12124=AXIS2_PLACEMENT_3D('',#19975,#15201,#15202);
#12125=AXIS2_PLACEMENT_3D('',#19976,#15203,#15204);
#12126=AXIS2_PLACEMENT_3D('',#19977,#15205,#15206);
#12127=AXIS2_PLACEMENT_3D('',#19978,#15207,#15208);
#12128=AXIS2_PLACEMENT_3D('',#19979,#15209,#15210);
#12129=AXIS2_PLACEMENT_3D('',#19980,#15211,#15212);
#12130=AXIS2_PLACEMENT_3D('',#19981,#15213,#15214);
#12131=AXIS2_PLACEMENT_3D('',#19982,#15215,#15216);
#12132=AXIS2_PLACEMENT_3D('',#19984,#15217,#15218);
#12133=AXIS2_PLACEMENT_3D('',#19987,#15220,#15221);
#12134=AXIS2_PLACEMENT_3D('',#19988,#15222,#15223);
#12135=AXIS2_PLACEMENT_3D('',#19990,#15224,#15225);
#12136=AXIS2_PLACEMENT_3D('',#19992,#15227,#15228);
#12137=AXIS2_PLACEMENT_3D('',#19994,#15229,#15230);
#12138=AXIS2_PLACEMENT_3D('',#19997,#15232,#15233);
#12139=AXIS2_PLACEMENT_3D('',#19998,#15234,#15235);
#12140=AXIS2_PLACEMENT_3D('',#20000,#15236,#15237);
#12141=AXIS2_PLACEMENT_3D('',#20002,#15239,#15240);
#12142=AXIS2_PLACEMENT_3D('',#20005,#15241,#15242);
#12143=AXIS2_PLACEMENT_3D('',#20009,#15244,#15245);
#12144=AXIS2_PLACEMENT_3D('',#20011,#15247,#15248);
#12145=AXIS2_PLACEMENT_3D('',#20014,#15249,#15250);
#12146=AXIS2_PLACEMENT_3D('',#20017,#15253,#15254);
#12147=AXIS2_PLACEMENT_3D('',#20020,#15255,#15256);
#12148=AXIS2_PLACEMENT_3D('',#20023,#15259,#15260);
#12149=AXIS2_PLACEMENT_3D('',#20026,#15263,#15264);
#12150=AXIS2_PLACEMENT_3D('',#20027,#15265,#15266);
#12151=AXIS2_PLACEMENT_3D('',#20028,#15267,#15268);
#12152=AXIS2_PLACEMENT_3D('',#20029,#15269,#15270);
#12153=AXIS2_PLACEMENT_3D('',#20034,#15272,#15273);
#12154=AXIS2_PLACEMENT_3D('',#20036,#15274,#15275);
#12155=AXIS2_PLACEMENT_3D('',#20038,#15276,#15277);
#12156=AXIS2_PLACEMENT_3D('',#20040,#15278,#15279);
#12157=AXIS2_PLACEMENT_3D('',#20042,#15280,#15281);
#12158=AXIS2_PLACEMENT_3D('',#20043,#15282,#15283);
#12159=AXIS2_PLACEMENT_3D('',#20044,#15284,#15285);
#12160=AXIS2_PLACEMENT_3D('',#20046,#15286,#15287);
#12161=AXIS2_PLACEMENT_3D('',#20048,#15288,#15289);
#12162=AXIS2_PLACEMENT_3D('',#20049,#15290,#15291);
#12163=AXIS2_PLACEMENT_3D('',#20050,#15292,#15293);
#12164=AXIS2_PLACEMENT_3D('',#20052,#15294,#15295);
#12165=AXIS2_PLACEMENT_3D('',#20055,#15297,#15298);
#12166=AXIS2_PLACEMENT_3D('',#20056,#15299,#15300);
#12167=AXIS2_PLACEMENT_3D('',#20058,#15302,#15303);
#12168=AXIS2_PLACEMENT_3D('',#20061,#15305,#15306);
#12169=AXIS2_PLACEMENT_3D('',#20062,#15307,#15308);
#12170=AXIS2_PLACEMENT_3D('',#20065,#15310,#15311);
#12171=AXIS2_PLACEMENT_3D('',#20066,#15312,#15313);
#12172=AXIS2_PLACEMENT_3D('',#20079,#15320,#15321);
#12173=AXIS2_PLACEMENT_3D('',#20080,#15322,#15323);
#12174=AXIS2_PLACEMENT_3D('',#20087,#15328,#15329);
#12175=AXIS2_PLACEMENT_3D('',#20092,#15333,#15334);
#12176=AXIS2_PLACEMENT_3D('',#20097,#15338,#15339);
#12177=AXIS2_PLACEMENT_3D('',#20102,#15343,#15344);
#12178=AXIS2_PLACEMENT_3D('',#20107,#15348,#15349);
#12179=AXIS2_PLACEMENT_3D('',#20110,#15352,#15353);
#12180=AXIS2_PLACEMENT_3D('',#20111,#15354,#15355);
#12181=AXIS2_PLACEMENT_3D('',#20112,#15356,#15357);
#12182=AXIS2_PLACEMENT_3D('',#20113,#15358,#15359);
#12183=AXIS2_PLACEMENT_3D('',#20114,#15360,#15361);
#12184=AXIS2_PLACEMENT_3D('',#20115,#15362,#15363);
#12185=AXIS2_PLACEMENT_3D('',#20116,#15364,#15365);
#12186=AXIS2_PLACEMENT_3D('',#20117,#15366,#15367);
#12187=AXIS2_PLACEMENT_3D('',#20118,#15368,#15369);
#12188=AXIS2_PLACEMENT_3D('',#20119,#15370,#15371);
#12189=AXIS2_PLACEMENT_3D('',#20120,#15372,#15373);
#12190=AXIS2_PLACEMENT_3D('',#20121,#15374,#15375);
#12191=AXIS2_PLACEMENT_3D('',#20122,#15376,#15377);
#12192=AXIS2_PLACEMENT_3D('',#20123,#15378,#15379);
#12193=AXIS2_PLACEMENT_3D('',#20124,#15380,#15381);
#12194=AXIS2_PLACEMENT_3D('',#20125,#15382,#15383);
#12195=AXIS2_PLACEMENT_3D('',#20126,#15384,#15385);
#12196=AXIS2_PLACEMENT_3D('',#20127,#15386,#15387);
#12197=AXIS2_PLACEMENT_3D('',#20128,#15388,#15389);
#12198=AXIS2_PLACEMENT_3D('',#20129,#15390,#15391);
#12199=AXIS2_PLACEMENT_3D('',#20130,#15392,#15393);
#12200=AXIS2_PLACEMENT_3D('',#20131,#15394,#15395);
#12201=AXIS2_PLACEMENT_3D('',#20132,#15396,#15397);
#12202=AXIS2_PLACEMENT_3D('',#20133,#15398,#15399);
#12203=AXIS2_PLACEMENT_3D('',#20134,#15400,#15401);
#12204=AXIS2_PLACEMENT_3D('',#20135,#15402,#15403);
#12205=AXIS2_PLACEMENT_3D('',#20136,#15404,#15405);
#12206=AXIS2_PLACEMENT_3D('',#20137,#15406,#15407);
#12207=AXIS2_PLACEMENT_3D('',#20138,#15408,#15409);
#12208=AXIS2_PLACEMENT_3D('',#20139,#15410,#15411);
#12209=AXIS2_PLACEMENT_3D('',#20140,#15412,#15413);
#12210=AXIS2_PLACEMENT_3D('',#20141,#15414,#15415);
#12211=AXIS2_PLACEMENT_3D('',#20142,#15416,#15417);
#12212=AXIS2_PLACEMENT_3D('',#20143,#15418,#15419);
#12213=AXIS2_PLACEMENT_3D('',#20144,#15420,#15421);
#12214=DIRECTION('axis',(0.,0.,1.));
#12215=DIRECTION('refdir',(1.,0.,0.));
#12216=DIRECTION('axis',(0.,0.,1.));
#12217=DIRECTION('refdir',(1.,0.,0.));
#12218=DIRECTION('center_axis',(0.,1.,0.));
#12219=DIRECTION('ref_axis',(0.,0.,1.));
#12220=DIRECTION('center_axis',(0.,1.,0.));
#12221=DIRECTION('ref_axis',(0.,0.,-1.));
#12222=DIRECTION('',(0.,1.,0.));
#12223=DIRECTION('center_axis',(0.,1.,0.));
#12224=DIRECTION('ref_axis',(0.,0.,1.));
#12225=DIRECTION('center_axis',(0.,1.,0.));
#12226=DIRECTION('ref_axis',(0.,0.,1.));
#12227=DIRECTION('center_axis',(0.,-1.,0.));
#12228=DIRECTION('ref_axis',(0.,0.,-1.));
#12229=DIRECTION('',(0.,1.,0.));
#12230=DIRECTION('center_axis',(0.,1.,0.));
#12231=DIRECTION('ref_axis',(0.,0.,-1.));
#12232=DIRECTION('center_axis',(0.,1.,0.));
#12233=DIRECTION('ref_axis',(0.,0.,1.));
#12234=DIRECTION('center_axis',(0.,1.,0.));
#12235=DIRECTION('ref_axis',(0.,0.,-1.));
#12236=DIRECTION('',(0.,1.,0.));
#12237=DIRECTION('center_axis',(0.,1.,0.));
#12238=DIRECTION('ref_axis',(0.,0.,1.));
#12239=DIRECTION('center_axis',(0.,1.,0.));
#12240=DIRECTION('ref_axis',(0.,0.,1.));
#12241=DIRECTION('center_axis',(0.,-1.,0.));
#12242=DIRECTION('ref_axis',(0.,0.,-1.));
#12243=DIRECTION('',(0.,1.,0.));
#12244=DIRECTION('center_axis',(0.,1.,0.));
#12245=DIRECTION('ref_axis',(0.,0.,-1.));
#12246=DIRECTION('center_axis',(0.,1.,0.));
#12247=DIRECTION('ref_axis',(0.,0.,1.));
#12248=DIRECTION('center_axis',(0.,1.,0.));
#12249=DIRECTION('ref_axis',(0.,0.,1.));
#12250=DIRECTION('',(0.,1.,0.));
#12251=DIRECTION('center_axis',(0.,1.,0.));
#12252=DIRECTION('ref_axis',(0.,0.,1.));
#12253=DIRECTION('center_axis',(0.,1.,0.));
#12254=DIRECTION('ref_axis',(0.,0.,1.));
#12255=DIRECTION('center_axis',(0.,-1.,0.));
#12256=DIRECTION('ref_axis',(0.,0.,-1.));
#12257=DIRECTION('',(0.,1.,0.));
#12258=DIRECTION('center_axis',(0.,1.,0.));
#12259=DIRECTION('ref_axis',(0.,0.,1.));
#12260=DIRECTION('center_axis',(0.,1.,0.));
#12261=DIRECTION('ref_axis',(0.,0.,1.));
#12262=DIRECTION('center_axis',(0.,1.,0.));
#12263=DIRECTION('ref_axis',(0.,0.,1.));
#12264=DIRECTION('',(0.,1.,0.));
#12265=DIRECTION('center_axis',(0.,1.,0.));
#12266=DIRECTION('ref_axis',(0.,0.,1.));
#12267=DIRECTION('center_axis',(0.,1.,0.));
#12268=DIRECTION('ref_axis',(0.,0.,1.));
#12269=DIRECTION('center_axis',(0.,-1.,0.));
#12270=DIRECTION('ref_axis',(0.,0.,-1.));
#12271=DIRECTION('',(0.,1.,0.));
#12272=DIRECTION('center_axis',(0.,1.,0.));
#12273=DIRECTION('ref_axis',(0.,0.,1.));
#12274=DIRECTION('center_axis',(-1.,-3.22196856956734E-16,0.));
#12275=DIRECTION('ref_axis',(3.22196856956734E-16,-1.,0.));
#12276=DIRECTION('center_axis',(1.,0.,0.));
#12277=DIRECTION('ref_axis',(0.,0.,-1.));
#12278=DIRECTION('',(-1.,-3.22196856956734E-16,0.));
#12279=DIRECTION('center_axis',(-1.,-3.22196856956734E-16,0.));
#12280=DIRECTION('ref_axis',(3.22196856956734E-16,-1.,0.));
#12281=DIRECTION('center_axis',(-1.,-3.22196856956734E-16,0.));
#12282=DIRECTION('ref_axis',(3.22196856956734E-16,-1.,0.));
#12283=DIRECTION('center_axis',(1.,0.,0.));
#12284=DIRECTION('ref_axis',(0.,0.,-1.));
#12285=DIRECTION('',(-1.,-3.22196856956734E-16,0.));
#12286=DIRECTION('center_axis',(-1.,-3.22196856956734E-16,0.));
#12287=DIRECTION('ref_axis',(3.22196856956734E-16,-1.,0.));
#12288=DIRECTION('center_axis',(-1.,-3.22196856956734E-16,0.));
#12289=DIRECTION('ref_axis',(3.22196856956734E-16,-1.,0.));
#12290=DIRECTION('center_axis',(1.,0.,0.));
#12291=DIRECTION('ref_axis',(0.,0.,-1.));
#12292=DIRECTION('',(-1.,-3.22196856956734E-16,0.));
#12293=DIRECTION('center_axis',(-1.,-3.22196856956734E-16,0.));
#12294=DIRECTION('ref_axis',(3.22196856956734E-16,-1.,0.));
#12295=DIRECTION('center_axis',(-1.,-3.22196856956734E-16,0.));
#12296=DIRECTION('ref_axis',(3.22196856956734E-16,-1.,0.));
#12297=DIRECTION('center_axis',(1.,0.,0.));
#12298=DIRECTION('ref_axis',(0.,0.,-1.));
#12299=DIRECTION('',(-1.,-3.22196856956734E-16,0.));
#12300=DIRECTION('center_axis',(-1.,-3.22196856956734E-16,0.));
#12301=DIRECTION('ref_axis',(3.22196856956734E-16,-1.,0.));
#12302=DIRECTION('center_axis',(-1.,-3.22196856956734E-16,0.));
#12303=DIRECTION('ref_axis',(3.22196856956734E-16,-1.,0.));
#12304=DIRECTION('center_axis',(1.,0.,0.));
#12305=DIRECTION('ref_axis',(0.,0.,-1.));
#12306=DIRECTION('',(-1.,-3.22196856956734E-16,0.));
#12307=DIRECTION('center_axis',(-1.,-3.22196856956734E-16,0.));
#12308=DIRECTION('ref_axis',(3.22196856956734E-16,-1.,0.));
#12309=DIRECTION('center_axis',(-1.,-3.22196856956734E-16,0.));
#12310=DIRECTION('ref_axis',(3.22196856956734E-16,-1.,0.));
#12311=DIRECTION('center_axis',(1.,0.,0.));
#12312=DIRECTION('ref_axis',(0.,0.,-1.));
#12313=DIRECTION('',(-1.,-3.22196856956734E-16,0.));
#12314=DIRECTION('center_axis',(-1.,-3.22196856956734E-16,0.));
#12315=DIRECTION('ref_axis',(3.22196856956734E-16,-1.,0.));
#12316=DIRECTION('center_axis',(-1.,-3.22196856956734E-16,0.));
#12317=DIRECTION('ref_axis',(3.22196856956734E-16,-1.,0.));
#12318=DIRECTION('center_axis',(1.,0.,0.));
#12319=DIRECTION('ref_axis',(0.,0.,-1.));
#12320=DIRECTION('',(-1.,-3.22196856956734E-16,0.));
#12321=DIRECTION('center_axis',(-1.,-3.22196856956734E-16,0.));
#12322=DIRECTION('ref_axis',(3.22196856956734E-16,-1.,0.));
#12323=DIRECTION('center_axis',(-1.,-3.22196856956734E-16,0.));
#12324=DIRECTION('ref_axis',(3.22196856956734E-16,-1.,0.));
#12325=DIRECTION('center_axis',(1.,0.,0.));
#12326=DIRECTION('ref_axis',(0.,0.,-1.));
#12327=DIRECTION('',(-1.,-3.22196856956734E-16,0.));
#12328=DIRECTION('center_axis',(-1.,-3.22196856956734E-16,0.));
#12329=DIRECTION('ref_axis',(3.22196856956734E-16,-1.,0.));
#12330=DIRECTION('center_axis',(-1.,-3.22196856956734E-16,0.));
#12331=DIRECTION('ref_axis',(3.22196856956734E-16,-1.,0.));
#12332=DIRECTION('center_axis',(1.,0.,0.));
#12333=DIRECTION('ref_axis',(0.,0.,-1.));
#12334=DIRECTION('',(-1.,-3.22196856956734E-16,0.));
#12335=DIRECTION('center_axis',(-1.,-3.22196856956734E-16,0.));
#12336=DIRECTION('ref_axis',(3.22196856956734E-16,-1.,0.));
#12337=DIRECTION('center_axis',(0.,0.,1.));
#12338=DIRECTION('ref_axis',(1.,0.,0.));
#12339=DIRECTION('',(-1.,0.,0.));
#12340=DIRECTION('center_axis',(0.,0.,1.));
#12341=DIRECTION('ref_axis',(-1.,0.,0.));
#12342=DIRECTION('',(-1.44560289664734E-16,-1.,0.));
#12343=DIRECTION('center_axis',(0.,0.,1.));
#12344=DIRECTION('ref_axis',(1.,0.,0.));
#12345=DIRECTION('center_axis',(0.,0.,1.));
#12346=DIRECTION('ref_axis',(1.,0.,0.));
#12347=DIRECTION('',(3.22196856956734E-16,-1.,0.));
#12348=DIRECTION('',(0.,-1.,0.));
#12349=DIRECTION('',(1.,0.,0.));
#12350=DIRECTION('center_axis',(0.,0.,-1.));
#12351=DIRECTION('ref_axis',(-1.,0.,0.));
#12352=DIRECTION('',(1.44560289664734E-16,1.,0.));
#12353=DIRECTION('center_axis',(0.,0.,1.));
#12354=DIRECTION('ref_axis',(-1.,0.,0.));
#12355=DIRECTION('',(1.,0.,0.));
#12356=DIRECTION('center_axis',(0.,0.,1.));
#12357=DIRECTION('ref_axis',(1.,0.,0.));
#12358=DIRECTION('center_axis',(0.,0.,-1.));
#12359=DIRECTION('ref_axis',(-1.,0.,0.));
#12360=DIRECTION('',(-1.,0.,0.));
#12361=DIRECTION('',(0.,-1.,0.));
#12362=DIRECTION('',(-1.,0.,0.));
#12363=DIRECTION('center_axis',(0.,0.,1.));
#12364=DIRECTION('ref_axis',(1.,0.,0.));
#12365=DIRECTION('',(0.,-1.,0.));
#12366=DIRECTION('center_axis',(0.,0.,1.));
#12367=DIRECTION('ref_axis',(-1.,-1.15648231731787E-15,0.));
#12368=DIRECTION('center_axis',(0.,0.,1.));
#12369=DIRECTION('ref_axis',(1.,0.,0.));
#12370=DIRECTION('center_axis',(0.,0.,1.));
#12371=DIRECTION('ref_axis',(1.,0.,0.));
#12372=DIRECTION('',(1.,0.,0.));
#12373=DIRECTION('',(0.,1.,0.));
#12374=DIRECTION('',(1.,0.,0.));
#12375=DIRECTION('center_axis',(0.,0.,-1.));
#12376=DIRECTION('ref_axis',(-1.,0.,0.));
#12377=DIRECTION('',(-1.,0.,0.));
#12378=DIRECTION('center_axis',(0.,0.,1.));
#12379=DIRECTION('ref_axis',(-1.,-1.15648231731787E-15,0.));
#12380=DIRECTION('',(0.,1.,0.));
#12381=DIRECTION('center_axis',(0.,0.,1.));
#12382=DIRECTION('ref_axis',(1.,0.,0.));
#12383=DIRECTION('center_axis',(0.,0.,-1.));
#12384=DIRECTION('ref_axis',(-1.,0.,0.));
#12385=DIRECTION('',(0.,-1.,0.));
#12386=DIRECTION('',(3.22196856956734E-16,-1.,0.));
#12387=DIRECTION('center_axis',(0.,1.,0.));
#12388=DIRECTION('ref_axis',(0.,0.,1.));
#12389=DIRECTION('',(-0.707106781186549,0.,0.707106781186547));
#12390=DIRECTION('center_axis',(0.,-1.,0.));
#12391=DIRECTION('ref_axis',(5.20417042793042E-15,0.,1.));
#12392=DIRECTION('',(0.,0.,-1.));
#12393=DIRECTION('',(1.,0.,0.));
#12394=DIRECTION('center_axis',(0.,-1.,0.));
#12395=DIRECTION('ref_axis',(0.,0.,1.));
#12396=DIRECTION('',(0.707106781186546,0.,0.707106781186549));
#12397=DIRECTION('center_axis',(0.,-1.,0.));
#12398=DIRECTION('ref_axis',(0.,0.,1.));
#12399=DIRECTION('',(0.,0.,-1.));
#12400=DIRECTION('center_axis',(0.,-1.,0.));
#12401=DIRECTION('ref_axis',(-1.31838984174237E-14,0.,1.));
#12402=DIRECTION('center_axis',(1.,0.,0.));
#12403=DIRECTION('ref_axis',(0.,0.,-1.));
#12404=DIRECTION('',(0.,0.,-1.));
#12405=DIRECTION('',(0.,-1.,0.));
#12406=DIRECTION('',(0.,1.,0.));
#12407=DIRECTION('center_axis',(0.,1.,0.));
#12408=DIRECTION('ref_axis',(0.,0.,1.));
#12409=DIRECTION('center_axis',(0.,1.,0.));
#12410=DIRECTION('ref_axis',(0.,0.,1.));
#12411=DIRECTION('',(0.707106781186549,0.,-0.707106781186547));
#12412=DIRECTION('center_axis',(0.,1.,0.));
#12413=DIRECTION('ref_axis',(0.,0.,1.));
#12414=DIRECTION('center_axis',(0.,1.,0.));
#12415=DIRECTION('ref_axis',(0.,0.,1.));
#12416=DIRECTION('',(-0.707106781186546,0.,-0.707106781186549));
#12417=DIRECTION('center_axis',(0.,1.,0.));
#12418=DIRECTION('ref_axis',(0.,0.,1.));
#12419=DIRECTION('',(1.,0.,0.));
#12420=DIRECTION('',(0.,0.,-1.));
#12421=DIRECTION('center_axis',(0.,0.,-1.));
#12422=DIRECTION('ref_axis',(-1.,0.,0.));
#12423=DIRECTION('',(0.,0.,-1.));
#12424=DIRECTION('center_axis',(1.,0.,0.));
#12425=DIRECTION('ref_axis',(0.,0.,-1.));
#12426=DIRECTION('',(0.,0.,-1.));
#12427=DIRECTION('center_axis',(0.,0.,-1.));
#12428=DIRECTION('ref_axis',(-1.,0.,0.));
#12429=DIRECTION('',(0.,0.,-1.));
#12430=DIRECTION('center_axis',(0.,-1.,0.));
#12431=DIRECTION('ref_axis',(0.,0.,-1.));
#12432=DIRECTION('center_axis',(0.,-1.,0.));
#12433=DIRECTION('ref_axis',(0.,0.,-1.));
#12434=DIRECTION('',(0.707106781186545,0.,0.70710678118655));
#12435=DIRECTION('center_axis',(0.,-1.,0.));
#12436=DIRECTION('ref_axis',(0.,0.,-1.));
#12437=DIRECTION('',(0.,0.,-1.));
#12438=DIRECTION('center_axis',(0.,-1.,0.));
#12439=DIRECTION('ref_axis',(0.,0.,-1.));
#12440=DIRECTION('',(-0.707106781186549,0.,0.707106781186547));
#12441=DIRECTION('center_axis',(0.,-1.,0.));
#12442=DIRECTION('ref_axis',(0.,0.,-1.));
#12443=DIRECTION('',(-1.,0.,0.));
#12444=DIRECTION('center_axis',(1.,0.,0.));
#12445=DIRECTION('ref_axis',(0.,0.,-1.));
#12446=DIRECTION('',(0.,1.,0.));
#12447=DIRECTION('',(0.,0.,-1.));
#12448=DIRECTION('',(0.,-1.,0.));
#12449=DIRECTION('center_axis',(0.,-1.,0.));
#12450=DIRECTION('ref_axis',(0.,0.,-1.));
#12451=DIRECTION('',(-0.707106781186545,0.,-0.70710678118655));
#12452=DIRECTION('center_axis',(0.,1.,0.));
#12453=DIRECTION('ref_axis',(1.04083408558608E-15,0.,-1.));
#12454=DIRECTION('',(0.,0.,-1.));
#12455=DIRECTION('',(-1.,0.,0.));
#12456=DIRECTION('center_axis',(0.,1.,0.));
#12457=DIRECTION('ref_axis',(5.20417042793042E-15,0.,-1.));
#12458=DIRECTION('',(0.707106781186549,0.,-0.707106781186546));
#12459=DIRECTION('center_axis',(0.,1.,0.));
#12460=DIRECTION('ref_axis',(-1.59594559789866E-14,0.,-1.));
#12461=DIRECTION('center_axis',(0.,1.,0.));
#12462=DIRECTION('ref_axis',(2.77555756156289E-15,0.,-1.));
#12463=DIRECTION('center_axis',(0.,0.,-1.));
#12464=DIRECTION('ref_axis',(-1.,0.,0.));
#12465=DIRECTION('',(0.,0.,-1.));
#12466=DIRECTION('center_axis',(1.,3.22196856956734E-16,0.));
#12467=DIRECTION('ref_axis',(-3.22196856956734E-16,1.,0.));
#12468=DIRECTION('',(0.,0.,-1.));
#12469=DIRECTION('center_axis',(0.,0.,-1.));
#12470=DIRECTION('ref_axis',(-1.,0.,0.));
#12471=DIRECTION('center_axis',(0.,0.,-1.));
#12472=DIRECTION('ref_axis',(-1.,0.,0.));
#12473=DIRECTION('',(0.,1.,0.));
#12474=DIRECTION('center_axis',(0.,0.,-1.));
#12475=DIRECTION('ref_axis',(-1.,0.,0.));
#12476=DIRECTION('',(0.,-1.,0.));
#12477=DIRECTION('center_axis',(-0.707106781186549,0.,0.707106781186546));
#12478=DIRECTION('ref_axis',(0.,-1.,0.));
#12479=DIRECTION('',(0.,-1.,0.));
#12480=DIRECTION('',(0.,1.,0.));
#12481=DIRECTION('center_axis',(-0.70710678118655,0.,0.707106781186545));
#12482=DIRECTION('ref_axis',(0.,-1.,0.));
#12483=DIRECTION('',(0.,1.,0.));
#12484=DIRECTION('',(0.,-1.,0.));
#12485=DIRECTION('center_axis',(-0.707106781186546,0.,-0.707106781186549));
#12486=DIRECTION('ref_axis',(0.,-1.,0.));
#12487=DIRECTION('',(0.,-1.,0.));
#12488=DIRECTION('',(0.,1.,0.));
#12489=DIRECTION('center_axis',(0.707106781186547,0.,0.707106781186548));
#12490=DIRECTION('ref_axis',(0.,1.,0.));
#12491=DIRECTION('',(0.,-1.,0.));
#12492=DIRECTION('',(0.,1.,0.));
#12493=DIRECTION('center_axis',(0.,-1.,0.));
#12494=DIRECTION('ref_axis',(0.,0.,-1.));
#12495=DIRECTION('center_axis',(0.,1.,0.));
#12496=DIRECTION('ref_axis',(0.,0.,1.));
#12497=DIRECTION('center_axis',(0.,-1.,0.));
#12498=DIRECTION('ref_axis',(0.,0.,-1.));
#12499=DIRECTION('center_axis',(0.,1.,0.));
#12500=DIRECTION('ref_axis',(0.,0.,1.));
#12501=DIRECTION('center_axis',(0.,1.,0.));
#12502=DIRECTION('ref_axis',(0.,0.,1.));
#12503=DIRECTION('center_axis',(0.,-1.,0.));
#12504=DIRECTION('ref_axis',(0.,0.,-1.));
#12505=DIRECTION('center_axis',(0.,-1.,0.));
#12506=DIRECTION('ref_axis',(0.,0.,-1.));
#12507=DIRECTION('center_axis',(0.,-1.,0.));
#12508=DIRECTION('ref_axis',(0.,0.,-1.));
#12509=DIRECTION('axis',(0.,0.,1.));
#12510=DIRECTION('refdir',(1.,0.,0.));
#12511=DIRECTION('center_axis',(0.,0.,1.));
#12512=DIRECTION('ref_axis',(1.,0.,0.));
#12513=DIRECTION('center_axis',(0.,0.,-1.));
#12514=DIRECTION('ref_axis',(1.,0.,0.));
#12515=DIRECTION('',(0.,0.,-1.));
#12516=DIRECTION('center_axis',(0.,0.,-1.));
#12517=DIRECTION('ref_axis',(1.,0.,0.));
#12518=DIRECTION('center_axis',(0.,0.,-1.));
#12519=DIRECTION('ref_axis',(-1.,0.,0.));
#12520=DIRECTION('center_axis',(0.,0.,1.));
#12521=DIRECTION('ref_axis',(-1.,0.,0.));
#12522=DIRECTION('',(0.,0.,1.));
#12523=DIRECTION('center_axis',(0.,0.,-1.));
#12524=DIRECTION('ref_axis',(-1.,0.,0.));
#12525=DIRECTION('center_axis',(0.,0.,-1.));
#12526=DIRECTION('ref_axis',(-1.,0.,0.));
#12527=DIRECTION('center_axis',(0.,0.,-1.));
#12528=DIRECTION('ref_axis',(-1.,0.,0.));
#12529=DIRECTION('',(0.,0.,-1.));
#12530=DIRECTION('center_axis',(0.,0.,-1.));
#12531=DIRECTION('ref_axis',(-1.,0.,0.));
#12532=DIRECTION('center_axis',(0.,0.,-1.));
#12533=DIRECTION('ref_axis',(-1.,0.,0.));
#12534=DIRECTION('center_axis',(0.,0.,-1.));
#12535=DIRECTION('ref_axis',(-1.,0.,0.));
#12536=DIRECTION('',(0.,0.,-1.));
#12537=DIRECTION('center_axis',(0.,0.,-1.));
#12538=DIRECTION('ref_axis',(-1.,0.,0.));
#12539=DIRECTION('center_axis',(0.,0.,-1.));
#12540=DIRECTION('ref_axis',(-1.,0.,0.));
#12541=DIRECTION('center_axis',(0.,0.,-1.));
#12542=DIRECTION('ref_axis',(-1.,0.,0.));
#12543=DIRECTION('',(0.,0.,-1.));
#12544=DIRECTION('center_axis',(0.,0.,-1.));
#12545=DIRECTION('ref_axis',(-1.,0.,0.));
#12546=DIRECTION('center_axis',(0.,0.,-1.));
#12547=DIRECTION('ref_axis',(-1.,0.,0.));
#12548=DIRECTION('center_axis',(0.,0.,-1.));
#12549=DIRECTION('ref_axis',(-1.,0.,0.));
#12550=DIRECTION('',(0.,0.,-1.));
#12551=DIRECTION('center_axis',(0.,0.,-1.));
#12552=DIRECTION('ref_axis',(-1.,0.,0.));
#12553=DIRECTION('center_axis',(0.,0.,-1.));
#12554=DIRECTION('ref_axis',(-1.,0.,0.));
#12555=DIRECTION('center_axis',(0.,0.,-1.));
#12556=DIRECTION('ref_axis',(-1.,0.,0.));
#12557=DIRECTION('',(0.,0.,-1.));
#12558=DIRECTION('center_axis',(0.,0.,-1.));
#12559=DIRECTION('ref_axis',(-1.,0.,0.));
#12560=DIRECTION('center_axis',(0.,0.,-1.));
#12561=DIRECTION('ref_axis',(-1.,0.,0.));
#12562=DIRECTION('center_axis',(0.,0.,-1.));
#12563=DIRECTION('ref_axis',(-1.,0.,0.));
#12564=DIRECTION('',(0.,0.,-1.));
#12565=DIRECTION('center_axis',(0.,0.,-1.));
#12566=DIRECTION('ref_axis',(-1.,0.,0.));
#12567=DIRECTION('center_axis',(0.,0.,-1.));
#12568=DIRECTION('ref_axis',(-1.,0.,0.));
#12569=DIRECTION('center_axis',(0.,0.,-1.));
#12570=DIRECTION('ref_axis',(-1.,0.,0.));
#12571=DIRECTION('',(0.,0.,-1.));
#12572=DIRECTION('center_axis',(0.,0.,1.));
#12573=DIRECTION('ref_axis',(-1.,0.,0.));
#12574=DIRECTION('center_axis',(0.,0.,-1.));
#12575=DIRECTION('ref_axis',(-1.,0.,0.));
#12576=DIRECTION('center_axis',(0.,0.,-1.));
#12577=DIRECTION('ref_axis',(-1.,0.,0.));
#12578=DIRECTION('',(0.,0.,-1.));
#12579=DIRECTION('center_axis',(0.,0.,1.));
#12580=DIRECTION('ref_axis',(-1.,0.,0.));
#12581=DIRECTION('center_axis',(0.,0.,-1.));
#12582=DIRECTION('ref_axis',(-1.,0.,0.));
#12583=DIRECTION('center_axis',(0.,0.,-1.));
#12584=DIRECTION('ref_axis',(-1.,0.,0.));
#12585=DIRECTION('',(0.,0.,-1.));
#12586=DIRECTION('center_axis',(0.,0.,1.));
#12587=DIRECTION('ref_axis',(-1.,0.,0.));
#12588=DIRECTION('center_axis',(0.,0.,-1.));
#12589=DIRECTION('ref_axis',(-1.,0.,0.));
#12590=DIRECTION('center_axis',(0.,0.,-1.));
#12591=DIRECTION('ref_axis',(-1.,0.,0.));
#12592=DIRECTION('',(0.,0.,-1.));
#12593=DIRECTION('center_axis',(0.,0.,1.));
#12594=DIRECTION('ref_axis',(-1.,0.,0.));
#12595=DIRECTION('center_axis',(0.,0.,-1.));
#12596=DIRECTION('ref_axis',(-1.,0.,0.));
#12597=DIRECTION('center_axis',(0.,0.,-1.));
#12598=DIRECTION('ref_axis',(-1.,0.,0.));
#12599=DIRECTION('',(0.,0.,-1.));
#12600=DIRECTION('center_axis',(0.,0.,1.));
#12601=DIRECTION('ref_axis',(-1.,0.,0.));
#12602=DIRECTION('center_axis',(0.,0.,-1.));
#12603=DIRECTION('ref_axis',(-1.,0.,0.));
#12604=DIRECTION('center_axis',(0.,0.,-1.));
#12605=DIRECTION('ref_axis',(-1.,0.,0.));
#12606=DIRECTION('',(0.,0.,-1.));
#12607=DIRECTION('center_axis',(0.,0.,1.));
#12608=DIRECTION('ref_axis',(-1.,0.,0.));
#12609=DIRECTION('center_axis',(0.,0.,-1.));
#12610=DIRECTION('ref_axis',(-1.,0.,0.));
#12611=DIRECTION('center_axis',(0.,0.,1.));
#12612=DIRECTION('ref_axis',(-1.,0.,0.));
#12613=DIRECTION('',(0.,0.,1.));
#12614=DIRECTION('center_axis',(0.,0.,-1.));
#12615=DIRECTION('ref_axis',(-1.,0.,0.));
#12616=DIRECTION('center_axis',(0.,0.,1.));
#12617=DIRECTION('ref_axis',(1.,0.,0.));
#12618=DIRECTION('center_axis',(0.,0.,-1.));
#12619=DIRECTION('ref_axis',(1.,0.,0.));
#12620=DIRECTION('',(0.,0.,1.));
#12621=DIRECTION('center_axis',(0.,0.,-1.));
#12622=DIRECTION('ref_axis',(1.,0.,0.));
#12623=DIRECTION('center_axis',(0.,0.,-1.));
#12624=DIRECTION('ref_axis',(-1.,0.,0.));
#12625=DIRECTION('center_axis',(0.,0.,1.));
#12626=DIRECTION('ref_axis',(-1.,0.,0.));
#12627=DIRECTION('',(0.,0.,1.));
#12628=DIRECTION('center_axis',(0.,0.,-1.));
#12629=DIRECTION('ref_axis',(-1.,0.,0.));
#12630=DIRECTION('center_axis',(0.,0.,1.));
#12631=DIRECTION('ref_axis',(1.,0.,0.));
#12632=DIRECTION('center_axis',(0.,0.,-1.));
#12633=DIRECTION('ref_axis',(1.,0.,0.));
#12634=DIRECTION('',(0.,0.,-1.));
#12635=DIRECTION('center_axis',(0.,0.,1.));
#12636=DIRECTION('ref_axis',(1.,0.,0.));
#12637=DIRECTION('center_axis',(0.,0.,-1.));
#12638=DIRECTION('ref_axis',(-1.,0.,0.));
#12639=DIRECTION('center_axis',(0.,0.,1.));
#12640=DIRECTION('ref_axis',(-1.,0.,0.));
#12641=DIRECTION('',(0.,0.,1.));
#12642=DIRECTION('center_axis',(0.,0.,-1.));
#12643=DIRECTION('ref_axis',(-1.,0.,0.));
#12644=DIRECTION('center_axis',(0.,0.,-1.));
#12645=DIRECTION('ref_axis',(-1.,0.,0.));
#12646=DIRECTION('center_axis',(0.,0.,1.));
#12647=DIRECTION('ref_axis',(-1.,0.,0.));
#12648=DIRECTION('',(0.,0.,1.));
#12649=DIRECTION('center_axis',(0.,0.,-1.));
#12650=DIRECTION('ref_axis',(-1.,0.,0.));
#12651=DIRECTION('center_axis',(0.,0.,-1.));
#12652=DIRECTION('ref_axis',(-1.,0.,0.));
#12653=DIRECTION('center_axis',(0.,0.,1.));
#12654=DIRECTION('ref_axis',(-1.,0.,0.));
#12655=DIRECTION('',(0.,0.,1.));
#12656=DIRECTION('center_axis',(0.,0.,1.));
#12657=DIRECTION('ref_axis',(-1.,0.,0.));
#12658=DIRECTION('center_axis',(0.,0.,-1.));
#12659=DIRECTION('ref_axis',(-1.,0.,0.));
#12660=DIRECTION('center_axis',(0.,0.,1.));
#12661=DIRECTION('ref_axis',(-1.,0.,0.));
#12662=DIRECTION('',(0.,0.,1.));
#12663=DIRECTION('center_axis',(0.,0.,1.));
#12664=DIRECTION('ref_axis',(-1.,0.,0.));
#12665=DIRECTION('center_axis',(0.,0.,1.));
#12666=DIRECTION('ref_axis',(1.,0.,0.));
#12667=DIRECTION('',(0.,1.,0.));
#12668=DIRECTION('',(-1.,0.,0.));
#12669=DIRECTION('',(0.,-1.,0.));
#12670=DIRECTION('',(1.,0.,0.));
#12671=DIRECTION('center_axis',(-1.,0.,0.));
#12672=DIRECTION('ref_axis',(0.,0.,1.));
#12673=DIRECTION('center_axis',(-1.,0.,0.));
#12674=DIRECTION('ref_axis',(0.,0.,1.));
#12675=DIRECTION('',(-1.,0.,0.));
#12676=DIRECTION('center_axis',(1.,0.,0.));
#12677=DIRECTION('ref_axis',(0.,2.04046848861772E-11,1.));
#12678=DIRECTION('center_axis',(0.,1.,0.));
#12679=DIRECTION('ref_axis',(0.,0.,1.));
#12680=DIRECTION('',(0.,1.,0.));
#12681=DIRECTION('center_axis',(0.,-1.,0.));
#12682=DIRECTION('ref_axis',(-1.10629098474627E-11,0.,1.));
#12683=DIRECTION('center_axis',(0.,1.,0.));
#12684=DIRECTION('ref_axis',(0.,0.,1.));
#12685=DIRECTION('center_axis',(1.,0.,0.));
#12686=DIRECTION('ref_axis',(0.,0.,-1.));
#12687=DIRECTION('',(1.,0.,0.));
#12688=DIRECTION('center_axis',(-1.,0.,0.));
#12689=DIRECTION('ref_axis',(0.,0.,-1.));
#12690=DIRECTION('center_axis',(1.,0.,0.));
#12691=DIRECTION('ref_axis',(0.,0.,-1.));
#12692=DIRECTION('center_axis',(0.,-1.,0.));
#12693=DIRECTION('ref_axis',(0.,0.,-1.));
#12694=DIRECTION('center_axis',(0.,-1.,0.));
#12695=DIRECTION('ref_axis',(0.,0.,-1.));
#12696=DIRECTION('',(0.,-1.,0.));
#12697=DIRECTION('center_axis',(0.,1.,0.));
#12698=DIRECTION('ref_axis',(-1.15648231731787E-15,0.,-1.));
#12699=DIRECTION('center_axis',(0.,0.,1.));
#12700=DIRECTION('ref_axis',(1.,0.,0.));
#12701=DIRECTION('center_axis',(0.,1.,0.));
#12702=DIRECTION('ref_axis',(0.,0.,1.));
#12703=DIRECTION('',(0.,0.,1.));
#12704=DIRECTION('',(-1.,0.,0.));
#12705=DIRECTION('',(0.,0.,-1.));
#12706=DIRECTION('',(-1.,0.,0.));
#12707=DIRECTION('',(0.,0.,-1.));
#12708=DIRECTION('',(-1.,0.,0.));
#12709=DIRECTION('',(0.,0.,-1.));
#12710=DIRECTION('',(-1.,0.,0.));
#12711=DIRECTION('',(-1.,0.,0.));
#12712=DIRECTION('',(-1.,0.,0.));
#12713=DIRECTION('',(0.,0.,1.));
#12714=DIRECTION('',(-1.,0.,0.));
#12715=DIRECTION('',(0.,0.,1.));
#12716=DIRECTION('',(-1.,0.,0.));
#12717=DIRECTION('',(0.,0.,1.));
#12718=DIRECTION('',(-1.,0.,0.));
#12719=DIRECTION('',(0.,0.,-1.));
#12720=DIRECTION('center_axis',(-1.,7.30644979272993E-12,1.28397990694513E-11));
#12721=DIRECTION('ref_axis',(1.28397990694513E-11,4.61084724568329E-27,
1.));
#12722=DIRECTION('center_axis',(1.28419072818016E-11,-4.85794204139804E-12,
1.));
#12723=DIRECTION('ref_axis',(1.,1.59160909755483E-27,-1.28419072818016E-11));
#12724=DIRECTION('center_axis',(1.,-6.33047047191158E-12,6.77618385437683E-12));
#12725=DIRECTION('ref_axis',(-6.77618385426471E-12,1.77115266899322E-11,
1.));
#12726=DIRECTION('center_axis',(-6.77562190498519E-12,5.3501387359779E-10,
1.));
#12727=DIRECTION('ref_axis',(1.95819442432296E-27,-1.,5.3501387359779E-10));
#12728=DIRECTION('center_axis',(1.,0.,0.));
#12729=DIRECTION('ref_axis',(0.,0.,-1.));
#12730=DIRECTION('',(0.,0.,-1.));
#12731=DIRECTION('',(0.,1.,0.));
#12732=DIRECTION('',(0.,0.,1.));
#12733=DIRECTION('center_axis',(0.,0.,1.));
#12734=DIRECTION('ref_axis',(1.,0.,0.));
#12735=DIRECTION('center_axis',(0.,-1.,0.));
#12736=DIRECTION('ref_axis',(0.,0.,-1.));
#12737=DIRECTION('',(0.,0.,1.));
#12738=DIRECTION('',(0.,0.,-1.));
#12739=DIRECTION('',(1.,0.,0.));
#12740=DIRECTION('center_axis',(0.,0.,1.));
#12741=DIRECTION('ref_axis',(1.,0.,0.));
#12742=DIRECTION('center_axis',(-1.,0.,0.));
#12743=DIRECTION('ref_axis',(0.,0.,1.));
#12744=DIRECTION('',(0.,0.,-1.));
#12745=DIRECTION('',(0.,-1.,0.));
#12746=DIRECTION('',(0.,0.,1.));
#12747=DIRECTION('center_axis',(0.,0.,-1.));
#12748=DIRECTION('ref_axis',(-1.,0.,0.));
#12749=DIRECTION('',(0.,0.,1.));
#12750=DIRECTION('center_axis',(0.,0.,-1.));
#12751=DIRECTION('ref_axis',(-1.,0.,0.));
#12752=DIRECTION('center_axis',(0.,0.,1.));
#12753=DIRECTION('ref_axis',(-1.,-1.73472347597681E-15,0.));
#12754=DIRECTION('center_axis',(0.,0.,-1.));
#12755=DIRECTION('ref_axis',(-1.,0.,0.));
#12756=DIRECTION('',(0.,0.,1.));
#12757=DIRECTION('center_axis',(0.,0.,-1.));
#12758=DIRECTION('ref_axis',(-1.,0.,0.));
#12759=DIRECTION('center_axis',(0.,0.,1.));
#12760=DIRECTION('ref_axis',(-1.,0.,0.));
#12761=DIRECTION('center_axis',(0.,0.,-1.));
#12762=DIRECTION('ref_axis',(-1.,0.,0.));
#12763=DIRECTION('',(0.,0.,1.));
#12764=DIRECTION('center_axis',(0.,0.,-1.));
#12765=DIRECTION('ref_axis',(-1.,0.,0.));
#12766=DIRECTION('center_axis',(0.,0.,1.));
#12767=DIRECTION('ref_axis',(-1.,-5.20417042793042E-15,0.));
#12768=DIRECTION('center_axis',(0.,0.,1.));
#12769=DIRECTION('ref_axis',(1.,0.,0.));
#12770=DIRECTION('',(0.,1.,0.));
#12771=DIRECTION('center_axis',(0.,0.,1.));
#12772=DIRECTION('ref_axis',(-1.,0.,0.));
#12773=DIRECTION('',(0.562310021407237,0.826926502069557,0.));
#12774=DIRECTION('center_axis',(0.,0.,1.));
#12775=DIRECTION('ref_axis',(-1.,-2.31296463463574E-15,0.));
#12776=DIRECTION('',(1.,0.,0.));
#12777=DIRECTION('center_axis',(0.,0.,1.));
#12778=DIRECTION('ref_axis',(-1.,2.31296463463574E-15,0.));
#12779=DIRECTION('',(0.562310021407237,-0.826926502069557,0.));
#12780=DIRECTION('center_axis',(0.,0.,1.));
#12781=DIRECTION('ref_axis',(-1.,0.,0.));
#12782=DIRECTION('',(0.,-1.,0.));
#12783=DIRECTION('center_axis',(0.,0.,1.));
#12784=DIRECTION('ref_axis',(-1.,-3.46944695195362E-15,0.));
#12785=DIRECTION('',(-0.562310021407322,-0.826926502069499,0.));
#12786=DIRECTION('center_axis',(6.0998774063795E-15,-4.61958004021261E-15,
-1.));
#12787=DIRECTION('ref_axis',(0.,1.,-4.44089209850062E-15));
#12788=DIRECTION('',(0.,1.,0.));
#12789=DIRECTION('center_axis',(0.,0.,1.));
#12790=DIRECTION('ref_axis',(-1.,0.,0.));
#12791=DIRECTION('',(1.,0.,0.));
#12792=DIRECTION('center_axis',(0.,0.,-1.));
#12793=DIRECTION('ref_axis',(-1.,0.,0.));
#12794=DIRECTION('',(0.,1.,0.));
#12795=DIRECTION('center_axis',(0.,0.,-1.));
#12796=DIRECTION('ref_axis',(1.,0.,0.));
#12797=DIRECTION('',(-1.,0.,0.));
#12798=DIRECTION('center_axis',(0.,0.,1.));
#12799=DIRECTION('ref_axis',(-1.,0.,0.));
#12800=DIRECTION('',(0.,1.,0.));
#12801=DIRECTION('center_axis',(0.,0.,-1.));
#12802=DIRECTION('ref_axis',(-1.,0.,0.));
#12803=DIRECTION('',(-1.,0.,0.));
#12804=DIRECTION('center_axis',(0.,0.,-1.));
#12805=DIRECTION('ref_axis',(1.,0.,0.));
#12806=DIRECTION('',(0.,-1.,0.));
#12807=DIRECTION('center_axis',(0.,0.,1.));
#12808=DIRECTION('ref_axis',(-1.,0.,0.));
#12809=DIRECTION('',(-1.,0.,0.));
#12810=DIRECTION('center_axis',(0.,0.,-1.));
#12811=DIRECTION('ref_axis',(-1.,0.,0.));
#12812=DIRECTION('',(0.,-1.,0.));
#12813=DIRECTION('center_axis',(0.,0.,-1.));
#12814=DIRECTION('ref_axis',(1.,-2.60208521396521E-15,0.));
#12815=DIRECTION('',(1.,0.,0.));
#12816=DIRECTION('center_axis',(0.,0.,1.));
#12817=DIRECTION('ref_axis',(-1.,0.,0.));
#12818=DIRECTION('',(0.,-1.,0.));
#12819=DIRECTION('center_axis',(0.,0.,-1.));
#12820=DIRECTION('ref_axis',(1.,4.4408920985006E-15,0.));
#12821=DIRECTION('center_axis',(0.,0.,1.));
#12822=DIRECTION('ref_axis',(-1.,-4.33680868994202E-15,0.));
#12823=DIRECTION('',(-0.562310021407322,0.826926502069499,0.));
#12824=DIRECTION('center_axis',(0.,0.,1.));
#12825=DIRECTION('ref_axis',(-1.,0.,0.));
#12826=DIRECTION('center_axis',(1.,0.,0.));
#12827=DIRECTION('ref_axis',(0.,0.,-1.));
#12828=DIRECTION('center_axis',(1.,0.,0.));
#12829=DIRECTION('ref_axis',(0.,0.,-1.));
#12830=DIRECTION('center_axis',(-1.,0.,0.));
#12831=DIRECTION('ref_axis',(0.,0.,-1.));
#12832=DIRECTION('',(-1.,0.,0.));
#12833=DIRECTION('center_axis',(0.,0.,-1.));
#12834=DIRECTION('ref_axis',(-1.,0.,0.));
#12835=DIRECTION('center_axis',(0.,0.,-1.));
#12836=DIRECTION('ref_axis',(-1.,0.,0.));
#12837=DIRECTION('',(0.,0.,-1.));
#12838=DIRECTION('center_axis',(0.,0.,-1.));
#12839=DIRECTION('ref_axis',(-1.,0.,0.));
#12840=DIRECTION('center_axis',(0.,0.,-1.));
#12841=DIRECTION('ref_axis',(-1.,0.,0.));
#12842=DIRECTION('',(0.,0.,-1.));
#12843=DIRECTION('center_axis',(0.,0.,1.));
#12844=DIRECTION('ref_axis',(-1.,0.,0.));
#12845=DIRECTION('center_axis',(0.,0.,-1.));
#12846=DIRECTION('ref_axis',(-1.,0.,0.));
#12847=DIRECTION('center_axis',(0.,0.,-1.));
#12848=DIRECTION('ref_axis',(-1.,0.,0.));
#12849=DIRECTION('',(0.,0.,-1.));
#12850=DIRECTION('center_axis',(0.,0.,1.));
#12851=DIRECTION('ref_axis',(-1.,0.,0.));
#12852=DIRECTION('center_axis',(0.,0.,-1.));
#12853=DIRECTION('ref_axis',(0.707106813086204,0.70710674928689,0.));
#12854=DIRECTION('center_axis',(0.,0.,1.));
#12855=DIRECTION('ref_axis',(-1.,0.,0.));
#12856=DIRECTION('center_axis',(0.,0.,1.));
#12857=DIRECTION('ref_axis',(1.,0.,0.));
#12858=DIRECTION('center_axis',(0.,0.,1.));
#12859=DIRECTION('ref_axis',(1.,0.,0.));
#12860=DIRECTION('center_axis',(0.,0.,1.));
#12861=DIRECTION('ref_axis',(1.,0.,0.));
#12862=DIRECTION('center_axis',(0.,0.,1.));
#12863=DIRECTION('ref_axis',(-1.,2.31296463463574E-15,0.));
#12864=DIRECTION('',(0.,1.,0.));
#12865=DIRECTION('center_axis',(0.,0.,1.));
#12866=DIRECTION('ref_axis',(-1.,0.,0.));
#12867=DIRECTION('',(-0.562310021407322,0.826926502069499,0.));
#12868=DIRECTION('center_axis',(0.,0.,-1.));
#12869=DIRECTION('ref_axis',(-1.,0.,0.));
#12870=DIRECTION('center_axis',(0.,0.,-1.));
#12871=DIRECTION('ref_axis',(-1.,0.,0.));
#12872=DIRECTION('',(-0.562310021407322,-0.826926502069499,0.));
#12873=DIRECTION('center_axis',(0.,0.,1.));
#12874=DIRECTION('ref_axis',(-1.,-3.46944695195362E-15,0.));
#12875=DIRECTION('',(0.,-1.,0.));
#12876=DIRECTION('center_axis',(0.,0.,1.));
#12877=DIRECTION('ref_axis',(-1.,0.,0.));
#12878=DIRECTION('',(0.562310021407237,-0.826926502069557,0.));
#12879=DIRECTION('center_axis',(0.,0.,1.));
#12880=DIRECTION('ref_axis',(-1.,2.31296463463574E-15,0.));
#12881=DIRECTION('',(1.,0.,0.));
#12882=DIRECTION('center_axis',(0.,0.,1.));
#12883=DIRECTION('ref_axis',(-1.,-2.31296463463574E-15,0.));
#12884=DIRECTION('',(0.562310021407237,0.826926502069557,0.));
#12885=DIRECTION('center_axis',(0.,0.,-1.));
#12886=DIRECTION('ref_axis',(-1.,0.,0.));
#12887=DIRECTION('center_axis',(3.41948691584553E-13,3.41948691584525E-13,
-1.));
#12888=DIRECTION('ref_axis',(-6.88338275267599E-14,-1.,-3.41948691584549E-13));
#12889=DIRECTION('center_axis',(0.,0.,-1.));
#12890=DIRECTION('ref_axis',(-1.,0.,0.));
#12891=DIRECTION('center_axis',(3.55271367880032E-13,-3.55271367880047E-13,
-1.));
#12892=DIRECTION('ref_axis',(-1.,7.10542735760108E-14,-3.55271367880054E-13));
#12893=DIRECTION('center_axis',(0.,0.,-1.));
#12894=DIRECTION('ref_axis',(-1.,0.,0.));
#12895=DIRECTION('center_axis',(-0.826926502069509,0.562310021407307,0.));
#12896=DIRECTION('ref_axis',(-0.562310021407307,-0.826926502069509,0.));
#12897=DIRECTION('',(0.,0.,1.));
#12898=DIRECTION('',(0.562310021410592,0.826926502067275,0.));
#12899=DIRECTION('',(0.,0.,1.));
#12900=DIRECTION('',(-0.562310021407307,-0.826926502069509,0.));
#12901=DIRECTION('',(0.,0.,-1.));
#12902=DIRECTION('',(-0.562310021407307,-0.826926502069509,0.));
#12903=DIRECTION('center_axis',(0.,0.,1.));
#12904=DIRECTION('ref_axis',(1.,0.,0.));
#12905=DIRECTION('',(0.,1.,0.));
#12906=DIRECTION('',(1.,0.,0.));
#12907=DIRECTION('center_axis',(-1.,0.,0.));
#12908=DIRECTION('ref_axis',(0.,0.,1.));
#12909=DIRECTION('',(0.,-1.,0.));
#12910=DIRECTION('',(0.,0.,1.));
#12911=DIRECTION('',(0.,1.,0.));
#12912=DIRECTION('',(0.,1.,0.));
#12913=DIRECTION('',(0.,0.,-1.));
#12914=DIRECTION('',(0.,1.,0.));
#12915=DIRECTION('',(0.,1.,0.));
#12916=DIRECTION('',(0.,1.,0.));
#12917=DIRECTION('',(0.,0.,1.));
#12918=DIRECTION('',(0.,1.,0.));
#12919=DIRECTION('',(0.,0.,-1.));
#12920=DIRECTION('',(0.,1.,0.));
#12921=DIRECTION('',(0.,1.,0.));
#12922=DIRECTION('',(0.,1.,0.));
#12923=DIRECTION('',(0.,0.,1.));
#12924=DIRECTION('',(0.,-1.,0.));
#12925=DIRECTION('',(0.,0.,1.));
#12926=DIRECTION('',(0.,-1.,0.));
#12927=DIRECTION('',(0.,-1.,0.));
#12928=DIRECTION('',(0.,-1.,0.));
#12929=DIRECTION('',(0.,0.,-1.));
#12930=DIRECTION('',(0.,-1.,0.));
#12931=DIRECTION('',(0.,0.,1.));
#12932=DIRECTION('',(0.,-1.,0.));
#12933=DIRECTION('',(0.,-1.,0.));
#12934=DIRECTION('',(0.,-1.,0.));
#12935=DIRECTION('',(0.,0.,1.));
#12936=DIRECTION('',(0.,-1.,0.));
#12937=DIRECTION('',(0.,0.,1.));
#12938=DIRECTION('',(0.,-1.,0.));
#12939=DIRECTION('',(0.,0.,-1.));
#12940=DIRECTION('',(0.,-1.,0.));
#12941=DIRECTION('',(0.,0.,-1.));
#12942=DIRECTION('',(0.,-1.,0.));
#12943=DIRECTION('',(0.,-1.,0.));
#12944=DIRECTION('',(0.,0.,1.));
#12945=DIRECTION('',(0.,1.,0.));
#12946=DIRECTION('',(0.,0.,1.));
#12947=DIRECTION('center_axis',(0.,0.,1.));
#12948=DIRECTION('ref_axis',(1.,0.,0.));
#12949=DIRECTION('',(-0.562310021407171,-0.826926502069602,0.));
#12950=DIRECTION('',(1.,0.,0.));
#12951=DIRECTION('center_axis',(0.826926502069509,-0.562310021407307,0.));
#12952=DIRECTION('ref_axis',(0.562310021407307,0.826926502069509,0.));
#12953=DIRECTION('',(0.562310021410592,0.826926502067275,0.));
#12954=DIRECTION('',(0.,0.,-1.));
#12955=DIRECTION('',(-0.562310021407307,-0.826926502069509,0.));
#12956=DIRECTION('',(0.,0.,1.));
#12957=DIRECTION('',(0.,0.,-1.));
#12958=DIRECTION('center_axis',(0.,0.,-1.));
#12959=DIRECTION('ref_axis',(-1.,0.,0.));
#12960=DIRECTION('',(0.,0.,1.));
#12961=DIRECTION('center_axis',(0.,0.,-1.));
#12962=DIRECTION('ref_axis',(-1.,0.,0.));
#12963=DIRECTION('',(0.,0.,-1.));
#12964=DIRECTION('center_axis',(-1.,0.,0.));
#12965=DIRECTION('ref_axis',(0.,0.,1.));
#12966=DIRECTION('',(0.,1.,0.));
#12967=DIRECTION('',(0.,0.,-1.));
#12968=DIRECTION('',(0.,1.,0.));
#12969=DIRECTION('',(0.,0.,1.));
#12970=DIRECTION('',(0.,1.,0.));
#12971=DIRECTION('',(0.,0.,-1.));
#12972=DIRECTION('',(0.,1.,0.));
#12973=DIRECTION('',(0.,0.,1.));
#12974=DIRECTION('',(0.,1.,0.));
#12975=DIRECTION('',(0.,0.,-1.));
#12976=DIRECTION('',(0.,1.,0.));
#12977=DIRECTION('',(0.,0.,1.));
#12978=DIRECTION('',(0.,1.,0.));
#12979=DIRECTION('',(0.,0.,1.));
#12980=DIRECTION('center_axis',(0.,0.,-1.));
#12981=DIRECTION('ref_axis',(-1.,0.,0.));
#12982=DIRECTION('center_axis',(0.,0.,-1.));
#12983=DIRECTION('ref_axis',(-1.,0.,0.));
#12984=DIRECTION('',(0.,0.,-1.));
#12985=DIRECTION('center_axis',(-0.826926502069509,0.562310021407307,0.));
#12986=DIRECTION('ref_axis',(-0.562310021407307,-0.826926502069509,0.));
#12987=DIRECTION('',(0.562310021407307,0.826926502069509,0.));
#12988=DIRECTION('',(0.,0.,1.));
#12989=DIRECTION('center_axis',(0.,0.,-1.));
#12990=DIRECTION('ref_axis',(-1.,0.,0.));
#12991=DIRECTION('center_axis',(0.,0.,-1.));
#12992=DIRECTION('ref_axis',(-1.,0.,0.));
#12993=DIRECTION('center_axis',(0.,0.,-1.));
#12994=DIRECTION('ref_axis',(-1.,0.,0.));
#12995=DIRECTION('',(0.,0.,-1.));
#12996=DIRECTION('center_axis',(0.,0.,-1.));
#12997=DIRECTION('ref_axis',(-1.,0.,0.));
#12998=DIRECTION('center_axis',(0.,1.,0.));
#12999=DIRECTION('ref_axis',(0.,0.,1.));
#13000=DIRECTION('',(1.,0.,0.));
#13001=DIRECTION('',(0.,0.,-1.));
#13002=DIRECTION('',(1.,0.,0.));
#13003=DIRECTION('',(0.,0.,1.));
#13004=DIRECTION('',(1.,0.,0.));
#13005=DIRECTION('',(0.,0.,-1.));
#13006=DIRECTION('',(1.,0.,0.));
#13007=DIRECTION('',(0.,0.,1.));
#13008=DIRECTION('',(1.,0.,0.));
#13009=DIRECTION('',(0.,0.,1.));
#13010=DIRECTION('center_axis',(0.,0.,-1.));
#13011=DIRECTION('ref_axis',(-1.,0.,0.));
#13012=DIRECTION('center_axis',(0.,0.,-1.));
#13013=DIRECTION('ref_axis',(-1.,0.,0.));
#13014=DIRECTION('center_axis',(0.,0.,-1.));
#13015=DIRECTION('ref_axis',(-1.,0.,0.));
#13016=DIRECTION('',(0.,0.,-1.));
#13017=DIRECTION('center_axis',(0.,0.,-1.));
#13018=DIRECTION('ref_axis',(-1.,0.,0.));
#13019=DIRECTION('center_axis',(0.826926502069509,0.562310021407307,0.));
#13020=DIRECTION('ref_axis',(-0.562310021407307,0.826926502069509,0.));
#13021=DIRECTION('',(0.562310021407307,-0.826926502069509,0.));
#13022=DIRECTION('',(0.,0.,1.));
#13023=DIRECTION('center_axis',(0.,0.,-1.));
#13024=DIRECTION('ref_axis',(-1.,0.,0.));
#13025=DIRECTION('center_axis',(0.,0.,-1.));
#13026=DIRECTION('ref_axis',(-1.,0.,0.));
#13027=DIRECTION('',(0.,0.,-1.));
#13028=DIRECTION('center_axis',(1.,0.,0.));
#13029=DIRECTION('ref_axis',(0.,0.,-1.));
#13030=DIRECTION('',(0.,-1.,0.));
#13031=DIRECTION('',(0.,0.,-1.));
#13032=DIRECTION('',(0.,-1.,0.));
#13033=DIRECTION('',(0.,0.,1.));
#13034=DIRECTION('',(0.,-1.,0.));
#13035=DIRECTION('',(0.,0.,-1.));
#13036=DIRECTION('',(0.,-1.,0.));
#13037=DIRECTION('',(0.,0.,1.));
#13038=DIRECTION('',(0.,-1.,0.));
#13039=DIRECTION('',(0.,0.,-1.));
#13040=DIRECTION('',(0.,-1.,0.));
#13041=DIRECTION('',(0.,0.,1.));
#13042=DIRECTION('',(0.,-1.,0.));
#13043=DIRECTION('',(0.,0.,1.));
#13044=DIRECTION('center_axis',(0.,0.,-1.));
#13045=DIRECTION('ref_axis',(-1.,0.,0.));
#13046=DIRECTION('center_axis',(0.,0.,-1.));
#13047=DIRECTION('ref_axis',(-1.,0.,0.));
#13048=DIRECTION('center_axis',(1.,9.94839377593602E-15,-1.10487024155554E-14));
#13049=DIRECTION('ref_axis',(-1.11656715619443E-14,0.,-1.));
#13050=DIRECTION('center_axis',(0.,1.,0.));
#13051=DIRECTION('ref_axis',(0.,0.,-1.));
#13052=DIRECTION('center_axis',(1.,-7.850462293419E-16,1.89526925396706E-15));
#13053=DIRECTION('ref_axis',(5.55111512312575E-16,1.,-6.6613381477509E-15));
#13054=DIRECTION('center_axis',(1.,0.,0.));
#13055=DIRECTION('ref_axis',(0.,0.,-1.));
#13056=DIRECTION('',(0.,1.,0.));
#13057=DIRECTION('',(0.,0.,-1.));
#13058=DIRECTION('center_axis',(0.,0.,-1.));
#13059=DIRECTION('ref_axis',(0.707106781233148,-0.707106781139947,0.));
#13060=DIRECTION('',(0.,0.,-1.));
#13061=DIRECTION('center_axis',(0.,0.,1.));
#13062=DIRECTION('ref_axis',(-1.,0.,0.));
#13063=DIRECTION('center_axis',(0.,-1.,0.));
#13064=DIRECTION('ref_axis',(0.,0.,-1.));
#13065=DIRECTION('',(0.,0.,-1.));
#13066=DIRECTION('',(1.,0.,0.));
#13067=DIRECTION('center_axis',(0.,0.,-1.));
#13068=DIRECTION('ref_axis',(-1.,0.,0.));
#13069=DIRECTION('center_axis',(-6.35468797035731E-9,6.35397964806342E-9,
-1.));
#13070=DIRECTION('ref_axis',(3.84137166520666E-13,1.,6.3539795647276E-9));
#13071=DIRECTION('',(0.,0.,1.));
#13072=DIRECTION('center_axis',(-1.,0.,0.));
#13073=DIRECTION('ref_axis',(0.,0.,1.));
#13074=DIRECTION('',(0.,-1.,0.));
#13075=DIRECTION('',(0.,0.,1.));
#13076=DIRECTION('center_axis',(0.,0.,1.));
#13077=DIRECTION('ref_axis',(1.,0.,0.));
#13078=DIRECTION('center_axis',(-6.36151393603232E-9,-6.36219561297833E-9,
-1.));
#13079=DIRECTION('ref_axis',(-1.,-5.67546010185474E-12,6.36151353813414E-9));
#13080=DIRECTION('',(0.,0.,1.));
#13081=DIRECTION('center_axis',(0.,1.,0.));
#13082=DIRECTION('ref_axis',(0.,0.,1.));
#13083=DIRECTION('',(0.,0.,-1.));
#13084=DIRECTION('',(-1.,0.,0.));
#13085=DIRECTION('center_axis',(0.,0.,-1.));
#13086=DIRECTION('ref_axis',(0.707106781233548,0.707106781139547,0.));
#13087=DIRECTION('',(0.,0.,-1.));
#13088=DIRECTION('center_axis',(0.,0.,1.));
#13089=DIRECTION('ref_axis',(-1.,0.,0.));
#13090=DIRECTION('center_axis',(1.,0.,0.));
#13091=DIRECTION('ref_axis',(0.,0.,-1.));
#13092=DIRECTION('',(0.,0.,-1.));
#13093=DIRECTION('',(0.,1.,0.));
#13094=DIRECTION('center_axis',(0.,0.,-1.));
#13095=DIRECTION('ref_axis',(-1.,0.,0.));
#13096=DIRECTION('center_axis',(-6.36152086670943E-9,-6.36220476409676E-9,
-1.));
#13097=DIRECTION('ref_axis',(-1.,3.73034936274398E-13,6.36152019951075E-9));
#13098=DIRECTION('',(0.,0.,1.));
#13099=DIRECTION('center_axis',(0.,-1.,0.));
#13100=DIRECTION('ref_axis',(0.,0.,-1.));
#13101=DIRECTION('',(1.,0.,0.));
#13102=DIRECTION('',(0.,0.,1.));
#13103=DIRECTION('center_axis',(0.,0.,1.));
#13104=DIRECTION('ref_axis',(1.,0.,0.));
#13105=DIRECTION('center_axis',(6.35475386807431E-9,-6.35404776622543E-9,
-1.));
#13106=DIRECTION('ref_axis',(5.99964522503824E-12,-1.,6.3540483985109E-9));
#13107=DIRECTION('',(0.,0.,1.));
#13108=DIRECTION('center_axis',(-1.,0.,0.));
#13109=DIRECTION('ref_axis',(0.,0.,1.));
#13110=DIRECTION('',(0.,0.,-1.));
#13111=DIRECTION('',(0.,-1.,0.));
#13112=DIRECTION('center_axis',(0.,0.,-1.));
#13113=DIRECTION('ref_axis',(-1.,0.,0.));
#13114=DIRECTION('',(0.,0.,-1.));
#13115=DIRECTION('center_axis',(0.,0.,1.));
#13116=DIRECTION('ref_axis',(-1.,0.,0.));
#13117=DIRECTION('center_axis',(0.,1.,0.));
#13118=DIRECTION('ref_axis',(0.,0.,1.));
#13119=DIRECTION('',(0.,0.,-1.));
#13120=DIRECTION('',(-1.,0.,0.));
#13121=DIRECTION('center_axis',(0.,0.,-1.));
#13122=DIRECTION('ref_axis',(-1.,0.,0.));
#13123=DIRECTION('center_axis',(6.35468797040853E-9,-6.35397964810999E-9,
-1.));
#13124=DIRECTION('ref_axis',(5.68434188605167E-12,-1.,6.35397956468904E-9));
#13125=DIRECTION('',(0.,0.,1.));
#13126=DIRECTION('center_axis',(1.,0.,0.));
#13127=DIRECTION('ref_axis',(0.,0.,-1.));
#13128=DIRECTION('',(0.,1.,0.));
#13129=DIRECTION('',(0.,0.,1.));
#13130=DIRECTION('center_axis',(0.,0.,1.));
#13131=DIRECTION('ref_axis',(1.,0.,0.));
#13132=DIRECTION('center_axis',(6.36153916910018E-9,6.36221862559652E-9,
-1.));
#13133=DIRECTION('ref_axis',(1.,6.00075544806287E-12,6.36154018348104E-9));
#13134=DIRECTION('',(0.,0.,1.));
#13135=DIRECTION('center_axis',(0.,-1.,0.));
#13136=DIRECTION('ref_axis',(0.,0.,-1.));
#13137=DIRECTION('',(0.,0.,-1.));
#13138=DIRECTION('',(1.,0.,0.));
#13139=DIRECTION('center_axis',(0.,0.,-1.));
#13140=DIRECTION('ref_axis',(-1.,0.,0.));
#13141=DIRECTION('',(0.,0.,-1.));
#13142=DIRECTION('center_axis',(0.,0.,1.));
#13143=DIRECTION('ref_axis',(-1.,0.,0.));
#13144=DIRECTION('center_axis',(-1.,0.,0.));
#13145=DIRECTION('ref_axis',(0.,0.,1.));
#13146=DIRECTION('',(0.,-1.,0.));
#13147=DIRECTION('center_axis',(-1.,-7.85046229341902E-16,1.89526925396706E-15));
#13148=DIRECTION('ref_axis',(-1.66533453693772E-15,6.66133814775089E-15,
-1.));
#13149=DIRECTION('center_axis',(1.,0.,0.));
#13150=DIRECTION('ref_axis',(0.,0.,-1.));
#13151=DIRECTION('center_axis',(0.,1.,0.));
#13152=DIRECTION('ref_axis',(0.,0.,-1.));
#13153=DIRECTION('center_axis',(-0.826926502069509,-0.562310021407307,0.));
#13154=DIRECTION('ref_axis',(0.562310021407307,-0.826926502069509,0.));
#13155=DIRECTION('',(-0.562310021407307,0.826926502069509,0.));
#13156=DIRECTION('',(0.,0.,-1.));
#13157=DIRECTION('',(-0.562310021407307,0.826926502069509,0.));
#13158=DIRECTION('',(0.,0.,1.));
#13159=DIRECTION('',(-0.562310021407307,0.826926502069509,0.));
#13160=DIRECTION('center_axis',(0.,0.,1.));
#13161=DIRECTION('ref_axis',(1.,0.,0.));
#13162=DIRECTION('center_axis',(-4.37239035198399E-13,-3.70337308189936E-13,
-1.));
#13163=DIRECTION('ref_axis',(-0.999999999999855,-5.39048211617437E-7,4.37168237134799E-13));
#13164=DIRECTION('',(-1.,0.,0.));
#13165=DIRECTION('',(0.,1.,0.));
#13166=DIRECTION('',(1.,0.,0.));
#13167=DIRECTION('center_axis',(-3.24372003830014E-13,4.24724639577507E-13,
-1.));
#13168=DIRECTION('ref_axis',(-4.6464532774625E-7,0.999999999999892,4.24480008512514E-13));
#13169=DIRECTION('',(0.,1.,0.));
#13170=DIRECTION('',(1.,0.,0.));
#13171=DIRECTION('',(0.,-1.,0.));
#13172=DIRECTION('center_axis',(3.95187814714554E-13,3.12137463243106E-13,
-1.));
#13173=DIRECTION('ref_axis',(0.999999999999951,3.13109078086861E-7,3.95643242527955E-13));
#13174=DIRECTION('',(1.,0.,0.));
#13175=DIRECTION('',(0.,-1.,0.));
#13176=DIRECTION('',(-1.,0.,0.));
#13177=DIRECTION('center_axis',(2.78474182098387E-15,-2.78474295664464E-15,
-1.));
#13178=DIRECTION('ref_axis',(-5.9452945013776E-7,-0.999999999999823,2.30695830588665E-15));
#13179=DIRECTION('',(0.,-1.,0.));
#13180=DIRECTION('',(0.,1.,0.));
#13181=DIRECTION('center_axis',(0.,0.,1.));
#13182=DIRECTION('ref_axis',(1.,0.,0.));
#13183=DIRECTION('',(1.,0.,0.));
#13184=DIRECTION('',(0.,-1.,0.));
#13185=DIRECTION('center_axis',(0.,0.,1.));
#13186=DIRECTION('ref_axis',(1.,0.,0.));
#13187=DIRECTION('',(-0.562310021407171,0.826926502069602,0.));
#13188=DIRECTION('',(1.,0.,0.));
#13189=DIRECTION('',(0.,-1.,0.));
#13190=DIRECTION('center_axis',(1.,0.,0.));
#13191=DIRECTION('ref_axis',(0.,0.,-1.));
#13192=DIRECTION('',(0.,0.,1.));
#13193=DIRECTION('',(0.,-1.,0.));
#13194=DIRECTION('',(0.,-1.,0.));
#13195=DIRECTION('',(0.,0.,-1.));
#13196=DIRECTION('',(0.,1.,0.));
#13197=DIRECTION('',(0.,0.,-1.));
#13198=DIRECTION('',(0.,-1.,0.));
#13199=DIRECTION('',(0.,0.,-1.));
#13200=DIRECTION('',(0.,1.,0.));
#13201=DIRECTION('',(0.,1.,0.));
#13202=DIRECTION('',(0.,0.,1.));
#13203=DIRECTION('',(0.,1.,0.));
#13204=DIRECTION('',(0.,0.,1.));
#13205=DIRECTION('',(0.,1.,0.));
#13206=DIRECTION('',(0.,0.,-1.));
#13207=DIRECTION('',(0.,1.,0.));
#13208=DIRECTION('',(0.,0.,-1.));
#13209=DIRECTION('',(0.,1.,0.));
#13210=DIRECTION('',(0.,1.,0.));
#13211=DIRECTION('',(0.,1.,0.));
#13212=DIRECTION('',(0.,0.,-1.));
#13213=DIRECTION('',(0.,1.,0.));
#13214=DIRECTION('',(0.,0.,1.));
#13215=DIRECTION('',(0.,1.,0.));
#13216=DIRECTION('',(0.,1.,0.));
#13217=DIRECTION('',(0.,1.,0.));
#13218=DIRECTION('',(0.,0.,-1.));
#13219=DIRECTION('',(0.,0.,-1.));
#13220=DIRECTION('',(0.,-1.,0.));
#13221=DIRECTION('',(0.,-1.,0.));
#13222=DIRECTION('',(0.,-1.,0.));
#13223=DIRECTION('',(0.,0.,1.));
#13224=DIRECTION('',(0.,-1.,0.));
#13225=DIRECTION('',(0.,0.,-1.));
#13226=DIRECTION('',(0.,-1.,0.));
#13227=DIRECTION('',(0.,-1.,0.));
#13228=DIRECTION('',(0.,-1.,0.));
#13229=DIRECTION('center_axis',(0.826926502069509,0.562310021407307,0.));
#13230=DIRECTION('ref_axis',(-0.562310021407307,0.826926502069509,0.));
#13231=DIRECTION('',(0.,0.,-1.));
#13232=DIRECTION('',(0.562310021410592,-0.826926502067275,0.));
#13233=DIRECTION('',(0.,0.,-1.));
#13234=DIRECTION('',(-0.562310021407307,0.826926502069509,0.));
#13235=DIRECTION('',(0.,0.,1.));
#13236=DIRECTION('center_axis',(1.,0.,0.));
#13237=DIRECTION('ref_axis',(0.,0.,-1.));
#13238=DIRECTION('',(0.,0.,1.));
#13239=DIRECTION('',(0.,1.,0.));
#13240=DIRECTION('',(0.,0.,1.));
#13241=DIRECTION('',(0.,0.,-1.));
#13242=DIRECTION('',(0.,1.,0.));
#13243=DIRECTION('',(0.,0.,-1.));
#13244=DIRECTION('',(0.,1.,0.));
#13245=DIRECTION('',(0.,0.,1.));
#13246=DIRECTION('',(0.,1.,0.));
#13247=DIRECTION('',(0.,0.,-1.));
#13248=DIRECTION('',(0.,1.,0.));
#13249=DIRECTION('',(0.,0.,1.));
#13250=DIRECTION('',(0.,1.,0.));
#13251=DIRECTION('',(0.,0.,-1.));
#13252=DIRECTION('',(0.,1.,0.));
#13253=DIRECTION('center_axis',(0.,0.,-1.));
#13254=DIRECTION('ref_axis',(-1.,0.,0.));
#13255=DIRECTION('',(0.,0.,-1.));
#13256=DIRECTION('center_axis',(0.,0.,1.));
#13257=DIRECTION('ref_axis',(-1.,4.62592926927149E-15,0.));
#13258=DIRECTION('center_axis',(0.826926502069509,-0.562310021407307,0.));
#13259=DIRECTION('ref_axis',(0.562310021407307,0.826926502069509,0.));
#13260=DIRECTION('',(0.,0.,-1.));
#13261=DIRECTION('',(0.562310021407307,0.826926502069509,0.));
#13262=DIRECTION('center_axis',(0.,0.,-1.));
#13263=DIRECTION('ref_axis',(-1.,0.,0.));
#13264=DIRECTION('',(0.,0.,-1.));
#13265=DIRECTION('center_axis',(0.,0.,1.));
#13266=DIRECTION('ref_axis',(-1.,0.,0.));
#13267=DIRECTION('center_axis',(0.,0.,1.));
#13268=DIRECTION('ref_axis',(-1.,-2.31296463463574E-15,0.));
#13269=DIRECTION('center_axis',(0.,0.,1.));
#13270=DIRECTION('ref_axis',(-1.,4.62592926927148E-15,0.));
#13271=DIRECTION('center_axis',(0.,-1.,0.));
#13272=DIRECTION('ref_axis',(0.,0.,-1.));
#13273=DIRECTION('',(0.,0.,1.));
#13274=DIRECTION('',(1.,0.,0.));
#13275=DIRECTION('',(0.,0.,-1.));
#13276=DIRECTION('',(1.,0.,0.));
#13277=DIRECTION('',(0.,0.,-1.));
#13278=DIRECTION('',(1.,0.,0.));
#13279=DIRECTION('',(0.,0.,1.));
#13280=DIRECTION('',(1.,0.,0.));
#13281=DIRECTION('',(0.,0.,-1.));
#13282=DIRECTION('',(1.,0.,0.));
#13283=DIRECTION('center_axis',(0.,0.,-1.));
#13284=DIRECTION('ref_axis',(-1.,0.,0.));
#13285=DIRECTION('',(0.,0.,-1.));
#13286=DIRECTION('center_axis',(0.,0.,1.));
#13287=DIRECTION('ref_axis',(-1.,0.,0.));
#13288=DIRECTION('center_axis',(0.,0.,1.));
#13289=DIRECTION('ref_axis',(-1.,0.,0.));
#13290=DIRECTION('center_axis',(0.,0.,1.));
#13291=DIRECTION('ref_axis',(-1.,0.,0.));
#13292=DIRECTION('center_axis',(-0.826926502069509,-0.562310021407307,0.));
#13293=DIRECTION('ref_axis',(0.562310021407307,-0.826926502069509,0.));
#13294=DIRECTION('',(0.,0.,-1.));
#13295=DIRECTION('',(0.562310021407307,-0.826926502069509,0.));
#13296=DIRECTION('center_axis',(0.,0.,-1.));
#13297=DIRECTION('ref_axis',(-1.,0.,0.));
#13298=DIRECTION('',(0.,0.,-1.));
#13299=DIRECTION('center_axis',(0.,0.,1.));
#13300=DIRECTION('ref_axis',(-1.,0.,0.));
#13301=DIRECTION('center_axis',(-1.,0.,0.));
#13302=DIRECTION('ref_axis',(0.,0.,1.));
#13303=DIRECTION('',(0.,0.,1.));
#13304=DIRECTION('',(0.,-1.,0.));
#13305=DIRECTION('',(0.,0.,-1.));
#13306=DIRECTION('',(0.,-1.,0.));
#13307=DIRECTION('',(0.,0.,-1.));
#13308=DIRECTION('',(0.,-1.,0.));
#13309=DIRECTION('',(0.,0.,1.));
#13310=DIRECTION('',(0.,-1.,0.));
#13311=DIRECTION('',(0.,0.,-1.));
#13312=DIRECTION('',(0.,-1.,0.));
#13313=DIRECTION('',(0.,0.,1.));
#13314=DIRECTION('',(0.,-1.,0.));
#13315=DIRECTION('',(0.,0.,-1.));
#13316=DIRECTION('',(0.,-1.,0.));
#13317=DIRECTION('center_axis',(0.,0.,-1.));
#13318=DIRECTION('ref_axis',(-1.,0.,0.));
#13319=DIRECTION('center_axis',(0.,0.,1.));
#13320=DIRECTION('ref_axis',(-1.,5.20417042793042E-15,0.));
#13321=DIRECTION('center_axis',(0.,0.,-1.));
#13322=DIRECTION('ref_axis',(-1.,0.,0.));
#13323=DIRECTION('center_axis',(0.,0.,1.));
#13324=DIRECTION('ref_axis',(-1.,1.73472347597681E-15,0.));
#13325=DIRECTION('center_axis',(0.,1.,0.));
#13326=DIRECTION('ref_axis',(0.,0.,1.));
#13327=DIRECTION('',(-1.,0.,0.));
#13328=DIRECTION('',(0.,0.,-1.));
#13329=DIRECTION('',(1.,0.,0.));
#13330=DIRECTION('center_axis',(0.,0.,1.));
#13331=DIRECTION('ref_axis',(1.,0.,0.));
#13332=DIRECTION('',(-1.,0.,0.));
#13333=DIRECTION('',(0.50000000000116,-0.866025403783769,0.));
#13334=DIRECTION('center_axis',(0.,1.,0.));
#13335=DIRECTION('ref_axis',(0.,0.,1.));
#13336=DIRECTION('center_axis',(0.,-1.,0.));
#13337=DIRECTION('ref_axis',(0.,0.,-1.));
#13338=DIRECTION('',(1.,0.,0.));
#13339=DIRECTION('',(0.,0.,1.));
#13340=DIRECTION('',(-1.,0.,0.));
#13341=DIRECTION('center_axis',(0.,0.,1.));
#13342=DIRECTION('ref_axis',(1.,0.,0.));
#13343=DIRECTION('',(0.866025403783496,0.500000000001632,0.));
#13344=DIRECTION('',(0.,1.,0.));
#13345=DIRECTION('center_axis',(0.,0.,-1.));
#13346=DIRECTION('ref_axis',(-1.,0.,0.));
#13347=DIRECTION('',(-1.,0.,0.));
#13348=DIRECTION('center_axis',(0.,0.,-1.));
#13349=DIRECTION('ref_axis',(-1.,0.,0.));
#13350=DIRECTION('',(0.,0.,1.));
#13351=DIRECTION('center_axis',(0.,0.,1.));
#13352=DIRECTION('ref_axis',(-1.,-3.46944695195361E-15,0.));
#13353=DIRECTION('center_axis',(0.,0.,1.));
#13354=DIRECTION('ref_axis',(1.,0.,0.));
#13355=DIRECTION('',(-1.,0.,0.));
#13356=DIRECTION('',(1.,0.,0.));
#13357=DIRECTION('',(0.,1.,0.));
#13358=DIRECTION('',(0.866025403783496,0.500000000001632,0.));
#13359=DIRECTION('center_axis',(0.,1.,0.));
#13360=DIRECTION('ref_axis',(0.,0.,1.));
#13361=DIRECTION('',(0.,0.,-1.));
#13362=DIRECTION('',(-1.,0.,0.));
#13363=DIRECTION('center_axis',(0.,0.,1.));
#13364=DIRECTION('ref_axis',(1.,0.,0.));
#13365=DIRECTION('center_axis',(0.,0.,1.));
#13366=DIRECTION('ref_axis',(1.,0.,0.));
#13367=DIRECTION('',(-1.,0.,0.));
#13368=DIRECTION('',(0.,1.,0.));
#13369=DIRECTION('',(-1.,0.,0.));
#13370=DIRECTION('center_axis',(0.,-1.,0.));
#13371=DIRECTION('ref_axis',(0.,0.,-1.));
#13372=DIRECTION('',(0.,0.,-1.));
#13373=DIRECTION('',(-1.,0.,0.));
#13374=DIRECTION('center_axis',(0.,-1.,0.));
#13375=DIRECTION('ref_axis',(0.,0.,-1.));
#13376=DIRECTION('',(-1.,0.,0.));
#13377=DIRECTION('',(0.,0.,1.));
#13378=DIRECTION('',(1.,0.,0.));
#13379=DIRECTION('center_axis',(0.,0.,1.));
#13380=DIRECTION('ref_axis',(1.,0.,0.));
#13381=DIRECTION('',(-1.,0.,0.));
#13382=DIRECTION('',(0.,1.,0.));
#13383=DIRECTION('center_axis',(0.,1.,0.));
#13384=DIRECTION('ref_axis',(0.,0.,1.));
#13385=DIRECTION('',(0.,0.,-1.));
#13386=DIRECTION('',(-1.,0.,0.));
#13387=DIRECTION('center_axis',(0.,1.,0.));
#13388=DIRECTION('ref_axis',(0.,0.,1.));
#13389=DIRECTION('',(0.,0.,1.));
#13390=DIRECTION('',(1.,0.,0.));
#13391=DIRECTION('',(-1.,0.,0.));
#13392=DIRECTION('center_axis',(0.,0.,1.));
#13393=DIRECTION('ref_axis',(1.,0.,0.));
#13394=DIRECTION('',(1.,0.,0.));
#13395=DIRECTION('',(0.,1.,0.));
#13396=DIRECTION('',(-0.500000000001634,-0.866025403783495,0.));
#13397=DIRECTION('',(-1.,0.,0.));
#13398=DIRECTION('center_axis',(0.,0.,-1.));
#13399=DIRECTION('ref_axis',(-1.,0.,0.));
#13400=DIRECTION('',(-0.500000000000017,0.866025403784429,0.));
#13401=DIRECTION('',(-0.499999999998097,-0.866025403785537,0.));
#13402=DIRECTION('center_axis',(0.,0.,1.));
#13403=DIRECTION('ref_axis',(1.,0.,0.));
#13404=DIRECTION('',(-1.,0.,0.));
#13405=DIRECTION('',(1.,0.,0.));
#13406=DIRECTION('',(0.500000000001634,-0.866025403783495,0.));
#13407=DIRECTION('center_axis',(0.,-1.,0.));
#13408=DIRECTION('ref_axis',(0.,0.,-1.));
#13409=DIRECTION('',(1.,0.,0.));
#13410=DIRECTION('center_axis',(0.,0.,1.));
#13411=DIRECTION('ref_axis',(1.,0.,0.));
#13412=DIRECTION('',(-1.,0.,0.));
#13413=DIRECTION('center_axis',(0.,1.,0.));
#13414=DIRECTION('ref_axis',(0.,0.,1.));
#13415=DIRECTION('',(1.,0.,0.));
#13416=DIRECTION('center_axis',(0.,0.,1.));
#13417=DIRECTION('ref_axis',(1.,0.,0.));
#13418=DIRECTION('',(-0.50000000000116,-0.866025403783769,0.));
#13419=DIRECTION('',(-1.,0.,0.));
#13420=DIRECTION('center_axis',(0.,0.,-1.));
#13421=DIRECTION('ref_axis',(-1.,0.,0.));
#13422=DIRECTION('',(-0.500000000000017,0.866025403784429,0.));
#13423=DIRECTION('',(-0.500000000009312,-0.866025403779062,0.));
#13424=DIRECTION('center_axis',(0.,0.,1.));
#13425=DIRECTION('ref_axis',(1.,0.,0.));
#13426=DIRECTION('',(-1.,0.,0.));
#13427=DIRECTION('',(1.,0.,0.));
#13428=DIRECTION('',(0.50000000000116,-0.866025403783769,0.));
#13429=DIRECTION('center_axis',(0.,-1.,0.));
#13430=DIRECTION('ref_axis',(0.,0.,-1.));
#13431=DIRECTION('center_axis',(0.,0.,-1.));
#13432=DIRECTION('ref_axis',(-1.,0.,0.));
#13433=DIRECTION('',(0.500000000000017,0.866025403784429,0.));
#13434=DIRECTION('',(0.500000000009309,-0.866025403779064,0.));
#13435=DIRECTION('center_axis',(0.,0.,1.));
#13436=DIRECTION('ref_axis',(1.,0.,0.));
#13437=DIRECTION('',(1.,0.,0.));
#13438=DIRECTION('',(-1.,0.,0.));
#13439=DIRECTION('',(-0.50000000000116,-0.866025403783769,0.));
#13440=DIRECTION('center_axis',(0.,-1.,0.));
#13441=DIRECTION('ref_axis',(0.,0.,-1.));
#13442=DIRECTION('',(-1.,0.,0.));
#13443=DIRECTION('center_axis',(0.,0.,1.));
#13444=DIRECTION('ref_axis',(1.,0.,0.));
#13445=DIRECTION('',(1.,0.,0.));
#13446=DIRECTION('center_axis',(0.,1.,0.));
#13447=DIRECTION('ref_axis',(0.,0.,1.));
#13448=DIRECTION('',(-1.,0.,0.));
#13449=DIRECTION('center_axis',(0.,0.,1.));
#13450=DIRECTION('ref_axis',(1.,0.,0.));
#13451=DIRECTION('',(0.500000000001634,-0.866025403783495,0.));
#13452=DIRECTION('',(1.,0.,0.));
#13453=DIRECTION('center_axis',(0.,0.,-1.));
#13454=DIRECTION('ref_axis',(-1.,0.,0.));
#13455=DIRECTION('',(0.500000000000017,0.866025403784429,0.));
#13456=DIRECTION('',(0.499999999998084,-0.866025403785545,0.));
#13457=DIRECTION('center_axis',(0.,0.,1.));
#13458=DIRECTION('ref_axis',(1.,0.,0.));
#13459=DIRECTION('',(1.,0.,0.));
#13460=DIRECTION('',(-1.,0.,0.));
#13461=DIRECTION('',(-0.500000000001634,-0.866025403783495,0.));
#13462=DIRECTION('center_axis',(0.,-1.,0.));
#13463=DIRECTION('ref_axis',(0.,0.,-1.));
#13464=DIRECTION('',(-1.,0.,0.));
#13465=DIRECTION('center_axis',(0.,0.,1.));
#13466=DIRECTION('ref_axis',(1.,0.,0.));
#13467=DIRECTION('center_axis',(0.,0.,1.));
#13468=DIRECTION('ref_axis',(1.,0.,0.));
#13469=DIRECTION('center_axis',(0.,-1.,0.));
#13470=DIRECTION('ref_axis',(0.,0.,-1.));
#13471=DIRECTION('',(0.,0.,1.));
#13472=DIRECTION('',(1.,0.,0.));
#13473=DIRECTION('center_axis',(0.,0.,-1.));
#13474=DIRECTION('ref_axis',(-1.,0.,0.));
#13475=DIRECTION('',(0.,-1.,0.));
#13476=DIRECTION('',(0.866025403783581,-0.500000000001486,0.));
#13477=DIRECTION('',(0.86602540378358,0.500000000001487,0.));
#13478=DIRECTION('',(0.,1.,0.));
#13479=DIRECTION('center_axis',(0.,0.,-1.));
#13480=DIRECTION('ref_axis',(-1.,0.,0.));
#13481=DIRECTION('',(1.,0.,0.));
#13482=DIRECTION('',(0.50000000000149,0.866025403783578,0.));
#13483=DIRECTION('',(-0.500000000001491,0.866025403783578,0.));
#13484=DIRECTION('',(-1.,0.,0.));
#13485=DIRECTION('center_axis',(0.,0.,-1.));
#13486=DIRECTION('ref_axis',(-1.,0.,0.));
#13487=DIRECTION('',(1.,0.,0.));
#13488=DIRECTION('',(0.50000000000149,0.866025403783578,0.));
#13489=DIRECTION('',(-0.50000000000149,0.866025403783578,0.));
#13490=DIRECTION('',(-1.,0.,0.));
#13491=DIRECTION('center_axis',(0.,0.,-1.));
#13492=DIRECTION('ref_axis',(-1.,0.,0.));
#13493=DIRECTION('',(0.,-1.,0.));
#13494=DIRECTION('',(0.86602540378358,-0.500000000001487,0.));
#13495=DIRECTION('',(0.866025403783581,0.500000000001486,0.));
#13496=DIRECTION('',(0.,1.,0.));
#13497=DIRECTION('center_axis',(0.,0.,-1.));
#13498=DIRECTION('ref_axis',(-1.,0.,0.));
#13499=DIRECTION('',(-1.,0.,0.));
#13500=DIRECTION('',(-0.500000000001491,-0.866025403783578,0.));
#13501=DIRECTION('',(0.50000000000149,-0.866025403783578,0.));
#13502=DIRECTION('',(1.,0.,0.));
#13503=DIRECTION('center_axis',(0.,0.,-1.));
#13504=DIRECTION('ref_axis',(-1.,0.,0.));
#13505=DIRECTION('',(-1.,0.,0.));
#13506=DIRECTION('',(-0.50000000000149,-0.866025403783578,0.));
#13507=DIRECTION('',(0.50000000000149,-0.866025403783578,0.));
#13508=DIRECTION('center_axis',(0.,1.,0.));
#13509=DIRECTION('ref_axis',(0.,0.,1.));
#13510=DIRECTION('',(0.,0.,1.));
#13511=DIRECTION('',(1.,0.,0.));
#13512=DIRECTION('center_axis',(0.,1.,0.));
#13513=DIRECTION('ref_axis',(0.,0.,1.));
#13514=DIRECTION('',(-1.,0.,0.));
#13515=DIRECTION('',(1.,0.,0.));
#13516=DIRECTION('center_axis',(0.,0.,1.));
#13517=DIRECTION('ref_axis',(1.,0.,0.));
#13518=DIRECTION('',(1.,0.,0.));
#13519=DIRECTION('center_axis',(0.,-1.,0.));
#13520=DIRECTION('ref_axis',(0.,0.,-1.));
#13521=DIRECTION('',(-1.,0.,0.));
#13522=DIRECTION('center_axis',(0.,-1.,0.));
#13523=DIRECTION('ref_axis',(0.,0.,-1.));
#13524=DIRECTION('',(0.,0.,-1.));
#13525=DIRECTION('',(-1.,0.,0.));
#13526=DIRECTION('center_axis',(0.,1.,0.));
#13527=DIRECTION('ref_axis',(0.,0.,1.));
#13528=DIRECTION('',(0.,0.,1.));
#13529=DIRECTION('',(1.,0.,0.));
#13530=DIRECTION('center_axis',(0.,1.,0.));
#13531=DIRECTION('ref_axis',(0.,0.,1.));
#13532=DIRECTION('',(-1.,0.,0.));
#13533=DIRECTION('',(1.,0.,0.));
#13534=DIRECTION('',(0.,0.,1.));
#13535=DIRECTION('center_axis',(0.,0.,1.));
#13536=DIRECTION('ref_axis',(1.,0.,0.));
#13537=DIRECTION('',(0.,-1.,0.));
#13538=DIRECTION('',(-1.,0.,0.));
#13539=DIRECTION('center_axis',(0.,0.,1.));
#13540=DIRECTION('ref_axis',(1.,0.,0.));
#13541=DIRECTION('',(1.,0.,0.));
#13542=DIRECTION('center_axis',(1.,0.,0.));
#13543=DIRECTION('ref_axis',(0.,0.,-1.));
#13544=DIRECTION('',(0.,0.,1.));
#13545=DIRECTION('',(0.,-1.,0.));
#13546=DIRECTION('center_axis',(1.,0.,0.));
#13547=DIRECTION('ref_axis',(0.,0.,-1.));
#13548=DIRECTION('',(0.,1.,0.));
#13549=DIRECTION('',(0.,-1.,0.));
#13550=DIRECTION('',(0.,0.,1.));
#13551=DIRECTION('center_axis',(0.,0.,1.));
#13552=DIRECTION('ref_axis',(1.,0.,0.));
#13553=DIRECTION('',(0.,-1.,0.));
#13554=DIRECTION('',(-1.,0.,0.));
#13555=DIRECTION('center_axis',(-1.,0.,0.));
#13556=DIRECTION('ref_axis',(0.,0.,1.));
#13557=DIRECTION('',(0.,1.,0.));
#13558=DIRECTION('',(0.,0.,-1.));
#13559=DIRECTION('center_axis',(-1.,0.,0.));
#13560=DIRECTION('ref_axis',(0.,0.,1.));
#13561=DIRECTION('',(0.,0.,-1.));
#13562=DIRECTION('',(0.,1.,0.));
#13563=DIRECTION('center_axis',(0.,1.,0.));
#13564=DIRECTION('ref_axis',(0.,0.,1.));
#13565=DIRECTION('',(0.,0.,-1.));
#13566=DIRECTION('center_axis',(0.,1.,0.));
#13567=DIRECTION('ref_axis',(0.,0.,1.));
#13568=DIRECTION('',(0.,0.,-1.));
#13569=DIRECTION('center_axis',(0.,-1.,0.));
#13570=DIRECTION('ref_axis',(0.,0.,-1.));
#13571=DIRECTION('',(0.,0.,1.));
#13572=DIRECTION('center_axis',(0.,1.,0.));
#13573=DIRECTION('ref_axis',(0.,0.,1.));
#13574=DIRECTION('',(0.,0.,-1.));
#13575=DIRECTION('center_axis',(0.,1.,0.));
#13576=DIRECTION('ref_axis',(0.,0.,1.));
#13577=DIRECTION('center_axis',(0.,1.,0.));
#13578=DIRECTION('ref_axis',(0.,0.,1.));
#13579=DIRECTION('center_axis',(1.63914506158791E-15,-4.24321088898506E-15,
-1.));
#13580=DIRECTION('ref_axis',(0.707106781281055,-0.70710678109204,4.64841042086043E-15));
#13581=DIRECTION('center_axis',(1.,1.83697019872103E-16,0.));
#13582=DIRECTION('ref_axis',(1.83697019872103E-16,-1.,0.));
#13583=DIRECTION('center_axis',(1.,0.,0.));
#13584=DIRECTION('ref_axis',(0.,0.,-1.));
#13585=DIRECTION('center_axis',(1.,0.,0.));
#13586=DIRECTION('ref_axis',(0.,0.,-1.));
#13587=DIRECTION('center_axis',(0.,1.,0.));
#13588=DIRECTION('ref_axis',(0.,0.,1.));
#13589=DIRECTION('center_axis',(0.,-1.,0.));
#13590=DIRECTION('ref_axis',(0.,0.,1.));
#13591=DIRECTION('center_axis',(0.,1.,0.));
#13592=DIRECTION('ref_axis',(0.,0.,1.));
#13593=DIRECTION('center_axis',(-1.,0.,0.));
#13594=DIRECTION('ref_axis',(0.,0.,1.));
#13595=DIRECTION('center_axis',(-1.,0.,0.));
#13596=DIRECTION('ref_axis',(0.,0.,1.));
#13597=DIRECTION('center_axis',(1.,0.,0.));
#13598=DIRECTION('ref_axis',(0.,0.,1.));
#13599=DIRECTION('center_axis',(1.48434289583302E-14,1.42898708586572E-14,
-1.));
#13600=DIRECTION('ref_axis',(0.707106781236163,0.707106781136932,2.0585817578096E-14));
#13601=DIRECTION('center_axis',(1.40259237217524E-10,1.,0.));
#13602=DIRECTION('ref_axis',(1.,-1.40259237217524E-10,0.));
#13603=DIRECTION('center_axis',(0.,1.,0.));
#13604=DIRECTION('ref_axis',(0.,0.,1.));
#13605=DIRECTION('center_axis',(0.,1.,0.));
#13606=DIRECTION('ref_axis',(0.,0.,1.));
#13607=DIRECTION('center_axis',(-1.,0.,0.));
#13608=DIRECTION('ref_axis',(0.,0.,1.));
#13609=DIRECTION('center_axis',(1.,0.,0.));
#13610=DIRECTION('ref_axis',(0.,0.,1.));
#13611=DIRECTION('center_axis',(-1.,0.,0.));
#13612=DIRECTION('ref_axis',(0.,0.,1.));
#13613=DIRECTION('center_axis',(0.,-1.,0.));
#13614=DIRECTION('ref_axis',(0.,0.,-1.));
#13615=DIRECTION('center_axis',(0.,-1.,0.));
#13616=DIRECTION('ref_axis',(0.,0.,-1.));
#13617=DIRECTION('center_axis',(0.,1.,0.));
#13618=DIRECTION('ref_axis',(0.,0.,-1.));
#13619=DIRECTION('center_axis',(1.17155445946046E-15,-2.64224536130632E-16,
-1.));
#13620=DIRECTION('ref_axis',(-1.,0.,-6.64058631551495E-16));
#13621=DIRECTION('center_axis',(-1.,1.40259742539074E-10,0.));
#13622=DIRECTION('ref_axis',(1.40259742539074E-10,1.,0.));
#13623=DIRECTION('center_axis',(-1.,0.,0.));
#13624=DIRECTION('ref_axis',(0.,0.,1.));
#13625=DIRECTION('center_axis',(-1.,0.,0.));
#13626=DIRECTION('ref_axis',(0.,0.,1.));
#13627=DIRECTION('center_axis',(0.,-1.,0.));
#13628=DIRECTION('ref_axis',(0.,0.,-1.));
#13629=DIRECTION('center_axis',(0.,1.,0.));
#13630=DIRECTION('ref_axis',(0.,0.,-1.));
#13631=DIRECTION('center_axis',(0.,-1.,0.));
#13632=DIRECTION('ref_axis',(0.,0.,-1.));
#13633=DIRECTION('center_axis',(1.,0.,0.));
#13634=DIRECTION('ref_axis',(0.,0.,-1.));
#13635=DIRECTION('center_axis',(1.,0.,0.));
#13636=DIRECTION('ref_axis',(0.,0.,-1.));
#13637=DIRECTION('center_axis',(-1.,0.,0.));
#13638=DIRECTION('ref_axis',(0.,0.,-1.));
#13639=DIRECTION('center_axis',(0.,0.,-1.));
#13640=DIRECTION('ref_axis',(-1.,0.,0.));
#13641=DIRECTION('center_axis',(0.,-1.,0.));
#13642=DIRECTION('ref_axis',(-1.,0.,0.));
#13643=DIRECTION('center_axis',(0.,-1.,0.));
#13644=DIRECTION('ref_axis',(0.,0.,-1.));
#13645=DIRECTION('center_axis',(0.,-1.,0.));
#13646=DIRECTION('ref_axis',(0.,0.,-1.));
#13647=DIRECTION('',(-1.,0.,0.));
#13648=DIRECTION('center_axis',(0.,0.,1.));
#13649=DIRECTION('ref_axis',(1.,0.,0.));
#13650=DIRECTION('',(0.50000000000116,0.866025403783769,0.));
#13651=DIRECTION('',(1.,0.,0.));
#13652=DIRECTION('center_axis',(0.,-1.,0.));
#13653=DIRECTION('ref_axis',(0.,0.,-1.));
#13654=DIRECTION('',(0.,0.,-1.));
#13655=DIRECTION('center_axis',(0.,1.,0.));
#13656=DIRECTION('ref_axis',(0.,0.,1.));
#13657=DIRECTION('',(-1.,0.,0.));
#13658=DIRECTION('center_axis',(0.,0.,1.));
#13659=DIRECTION('ref_axis',(1.,0.,0.));
#13660=DIRECTION('',(-1.,0.,0.));
#13661=DIRECTION('center_axis',(0.,-1.,0.));
#13662=DIRECTION('ref_axis',(0.,0.,-1.));
#13663=DIRECTION('',(1.,0.,0.));
#13664=DIRECTION('center_axis',(0.,0.,1.));
#13665=DIRECTION('ref_axis',(1.,0.,0.));
#13666=DIRECTION('',(-0.500000000001634,0.866025403783495,0.));
#13667=DIRECTION('',(-1.,0.,0.));
#13668=DIRECTION('center_axis',(0.,0.,-1.));
#13669=DIRECTION('ref_axis',(-1.,0.,0.));
#13670=DIRECTION('',(-0.500000000000017,-0.866025403784429,0.));
#13671=DIRECTION('',(-0.499999999998097,0.866025403785537,0.));
#13672=DIRECTION('center_axis',(0.,0.,1.));
#13673=DIRECTION('ref_axis',(1.,0.,0.));
#13674=DIRECTION('',(-1.,0.,0.));
#13675=DIRECTION('',(1.,0.,0.));
#13676=DIRECTION('',(0.500000000001634,0.866025403783495,0.));
#13677=DIRECTION('center_axis',(0.,1.,0.));
#13678=DIRECTION('ref_axis',(0.,0.,1.));
#13679=DIRECTION('',(1.,0.,0.));
#13680=DIRECTION('center_axis',(0.,0.,1.));
#13681=DIRECTION('ref_axis',(1.,0.,0.));
#13682=DIRECTION('',(-1.,0.,0.));
#13683=DIRECTION('center_axis',(0.,-1.,0.));
#13684=DIRECTION('ref_axis',(0.,0.,-1.));
#13685=DIRECTION('',(1.,0.,0.));
#13686=DIRECTION('center_axis',(0.,0.,1.));
#13687=DIRECTION('ref_axis',(1.,0.,0.));
#13688=DIRECTION('',(-0.50000000000116,0.866025403783769,0.));
#13689=DIRECTION('',(-1.,0.,0.));
#13690=DIRECTION('center_axis',(0.,0.,-1.));
#13691=DIRECTION('ref_axis',(-1.,0.,0.));
#13692=DIRECTION('',(-0.500000000000017,-0.866025403784429,0.));
#13693=DIRECTION('',(-0.500000000009312,0.866025403779062,0.));
#13694=DIRECTION('center_axis',(0.,0.,1.));
#13695=DIRECTION('ref_axis',(1.,0.,0.));
#13696=DIRECTION('',(1.,0.,0.));
#13697=DIRECTION('',(0.50000000000116,0.866025403783769,0.));
#13698=DIRECTION('center_axis',(0.,0.,-1.));
#13699=DIRECTION('ref_axis',(-1.,0.,0.));
#13700=DIRECTION('',(-0.500000000009312,0.866025403779062,0.));
#13701=DIRECTION('',(0.500000000009309,0.866025403779064,0.));
#13702=DIRECTION('center_axis',(0.,0.,1.));
#13703=DIRECTION('ref_axis',(1.,0.,0.));
#13704=DIRECTION('',(-0.50000000000116,0.866025403783769,0.));
#13705=DIRECTION('center_axis',(0.,0.,1.));
#13706=DIRECTION('ref_axis',(1.,0.,0.));
#13707=DIRECTION('',(0.500000000001634,0.866025403783495,0.));
#13708=DIRECTION('center_axis',(0.,0.,-1.));
#13709=DIRECTION('ref_axis',(-1.,0.,0.));
#13710=DIRECTION('',(-0.499999999998097,0.866025403785537,0.));
#13711=DIRECTION('',(0.499999999998084,0.866025403785545,0.));
#13712=DIRECTION('center_axis',(0.,0.,1.));
#13713=DIRECTION('ref_axis',(1.,0.,0.));
#13714=DIRECTION('',(-0.500000000001634,0.866025403783495,0.));
#13715=DIRECTION('',(1.,0.,0.));
#13716=DIRECTION('',(0.,-1.,0.));
#13717=DIRECTION('center_axis',(0.,1.,0.));
#13718=DIRECTION('ref_axis',(0.,0.,1.));
#13719=DIRECTION('',(0.,0.,-1.));
#13720=DIRECTION('',(1.,0.,0.));
#13721=DIRECTION('center_axis',(0.,1.,0.));
#13722=DIRECTION('ref_axis',(0.,0.,1.));
#13723=DIRECTION('',(1.,0.,0.));
#13724=DIRECTION('',(0.,0.,1.));
#13725=DIRECTION('',(-1.,0.,0.));
#13726=DIRECTION('center_axis',(0.,0.,1.));
#13727=DIRECTION('ref_axis',(1.,0.,0.));
#13728=DIRECTION('',(1.,0.,0.));
#13729=DIRECTION('',(0.,-1.,0.));
#13730=DIRECTION('center_axis',(0.,-1.,0.));
#13731=DIRECTION('ref_axis',(0.,0.,-1.));
#13732=DIRECTION('',(0.,0.,-1.));
#13733=DIRECTION('',(1.,0.,0.));
#13734=DIRECTION('center_axis',(0.,-1.,0.));
#13735=DIRECTION('ref_axis',(0.,0.,-1.));
#13736=DIRECTION('',(0.,0.,1.));
#13737=DIRECTION('',(-1.,0.,0.));
#13738=DIRECTION('center_axis',(0.,1.,0.));
#13739=DIRECTION('ref_axis',(0.,0.,1.));
#13740=DIRECTION('',(1.,0.,0.));
#13741=DIRECTION('',(0.,0.,1.));
#13742=DIRECTION('center_axis',(0.,0.,1.));
#13743=DIRECTION('ref_axis',(1.,0.,0.));
#13744=DIRECTION('center_axis',(0.,0.,-1.));
#13745=DIRECTION('ref_axis',(-1.,0.,0.));
#13746=DIRECTION('',(-1.,0.,0.));
#13747=DIRECTION('',(0.866025403783496,-0.500000000001632,0.));
#13748=DIRECTION('',(0.,-1.,0.));
#13749=DIRECTION('center_axis',(0.,0.,-1.));
#13750=DIRECTION('ref_axis',(-1.,0.,0.));
#13751=DIRECTION('center_axis',(0.,0.,-1.));
#13752=DIRECTION('ref_axis',(-1.,0.,0.));
#13753=DIRECTION('',(0.,0.,-1.));
#13754=DIRECTION('center_axis',(0.,0.,1.));
#13755=DIRECTION('ref_axis',(1.,0.,0.));
#13756=DIRECTION('',(1.,0.,0.));
#13757=DIRECTION('',(0.,-1.,0.));
#13758=DIRECTION('',(0.866025403783496,-0.500000000001632,0.));
#13759=DIRECTION('',(-1.,0.,0.));
#13760=DIRECTION('center_axis',(0.,-1.,0.));
#13761=DIRECTION('ref_axis',(0.,0.,-1.));
#13762=DIRECTION('',(-1.,0.,0.));
#13763=DIRECTION('',(0.,0.,-1.));
#13764=DIRECTION('center_axis',(0.,0.,1.));
#13765=DIRECTION('ref_axis',(1.,0.,0.));
#13766=DIRECTION('center_axis',(0.,1.,0.));
#13767=DIRECTION('ref_axis',(0.,0.,1.));
#13768=DIRECTION('',(1.,0.,0.));
#13769=DIRECTION('',(0.,0.,1.));
#13770=DIRECTION('center_axis',(0.,0.,-1.));
#13771=DIRECTION('ref_axis',(-1.,0.,0.));
#13772=DIRECTION('',(0.,-1.,0.));
#13773=DIRECTION('',(0.,1.,0.));
#13774=DIRECTION('',(0.86602540378358,0.500000000001487,0.));
#13775=DIRECTION('',(0.866025403783581,-0.500000000001486,0.));
#13776=DIRECTION('center_axis',(0.,0.,-1.));
#13777=DIRECTION('ref_axis',(-1.,0.,0.));
#13778=DIRECTION('',(0.50000000000149,0.866025403783578,0.));
#13779=DIRECTION('',(1.,0.,0.));
#13780=DIRECTION('',(-1.,0.,0.));
#13781=DIRECTION('',(-0.500000000001491,0.866025403783578,0.));
#13782=DIRECTION('center_axis',(0.,0.,-1.));
#13783=DIRECTION('ref_axis',(-1.,0.,0.));
#13784=DIRECTION('',(-1.,0.,0.));
#13785=DIRECTION('',(-0.50000000000149,0.866025403783578,0.));
#13786=DIRECTION('',(0.50000000000149,0.866025403783578,0.));
#13787=DIRECTION('center_axis',(0.,0.,-1.));
#13788=DIRECTION('ref_axis',(-1.,0.,0.));
#13789=DIRECTION('',(0.,-1.,0.));
#13790=DIRECTION('',(0.,1.,0.));
#13791=DIRECTION('',(0.866025403783581,0.500000000001486,0.));
#13792=DIRECTION('',(0.86602540378358,-0.500000000001487,0.));
#13793=DIRECTION('center_axis',(0.,0.,-1.));
#13794=DIRECTION('ref_axis',(-1.,0.,0.));
#13795=DIRECTION('',(-0.500000000001491,-0.866025403783578,0.));
#13796=DIRECTION('',(-1.,0.,0.));
#13797=DIRECTION('',(1.,0.,0.));
#13798=DIRECTION('',(0.50000000000149,-0.866025403783578,0.));
#13799=DIRECTION('center_axis',(0.,0.,-1.));
#13800=DIRECTION('ref_axis',(-1.,0.,0.));
#13801=DIRECTION('',(-1.,0.,0.));
#13802=DIRECTION('',(0.50000000000149,-0.866025403783578,0.));
#13803=DIRECTION('',(-0.50000000000149,-0.866025403783578,0.));
#13804=DIRECTION('center_axis',(0.,-1.,0.));
#13805=DIRECTION('ref_axis',(0.,0.,-1.));
#13806=DIRECTION('',(0.,0.,-1.));
#13807=DIRECTION('center_axis',(0.,1.,0.));
#13808=DIRECTION('ref_axis',(0.,0.,1.));
#13809=DIRECTION('',(0.,0.,1.));
#13810=DIRECTION('center_axis',(0.,-1.,0.));
#13811=DIRECTION('ref_axis',(0.,0.,-1.));
#13812=DIRECTION('',(0.,0.,-1.));
#13813=DIRECTION('center_axis',(-1.,0.,0.));
#13814=DIRECTION('ref_axis',(0.,0.,1.));
#13815=DIRECTION('',(0.,-1.,0.));
#13816=DIRECTION('',(0.,0.,-1.));
#13817=DIRECTION('center_axis',(-1.,0.,0.));
#13818=DIRECTION('ref_axis',(0.,0.,1.));
#13819=DIRECTION('',(0.,1.,0.));
#13820=DIRECTION('',(0.,0.,-1.));
#13821=DIRECTION('',(0.,-1.,0.));
#13822=DIRECTION('center_axis',(0.,0.,1.));
#13823=DIRECTION('ref_axis',(1.,0.,0.));
#13824=DIRECTION('',(0.,-1.,0.));
#13825=DIRECTION('',(-1.,0.,0.));
#13826=DIRECTION('center_axis',(1.,0.,0.));
#13827=DIRECTION('ref_axis',(0.,0.,-1.));
#13828=DIRECTION('',(0.,1.,0.));
#13829=DIRECTION('',(0.,0.,1.));
#13830=DIRECTION('center_axis',(1.,0.,0.));
#13831=DIRECTION('ref_axis',(0.,0.,-1.));
#13832=DIRECTION('',(0.,0.,1.));
#13833=DIRECTION('',(0.,1.,0.));
#13834=DIRECTION('center_axis',(0.,-1.,0.));
#13835=DIRECTION('ref_axis',(0.,0.,-1.));
#13836=DIRECTION('',(0.,0.,1.));
#13837=DIRECTION('center_axis',(0.,1.,0.));
#13838=DIRECTION('ref_axis',(0.,0.,1.));
#13839=DIRECTION('',(0.,0.,-1.));
#13840=DIRECTION('center_axis',(0.,-1.,0.));
#13841=DIRECTION('ref_axis',(0.,0.,-1.));
#13842=DIRECTION('',(0.,0.,1.));
#13843=DIRECTION('center_axis',(0.,0.,-1.));
#13844=DIRECTION('ref_axis',(-1.,0.,0.));
#13845=DIRECTION('center_axis',(0.866025403784429,0.500000000000017,0.));
#13846=DIRECTION('ref_axis',(-0.500000000000017,0.866025403784429,0.));
#13847=DIRECTION('',(0.,0.,-1.));
#13848=DIRECTION('center_axis',(-1.,0.,0.));
#13849=DIRECTION('ref_axis',(0.,0.,1.));
#13850=DIRECTION('',(0.,0.,-1.));
#13851=DIRECTION('center_axis',(-0.500000000000017,0.866025403784429,0.));
#13852=DIRECTION('ref_axis',(-0.866025403784429,-0.500000000000017,0.));
#13853=DIRECTION('',(-0.866025403784429,-0.500000000000017,0.));
#13854=DIRECTION('',(0.,0.,-1.));
#13855=DIRECTION('center_axis',(0.,-1.,0.));
#13856=DIRECTION('ref_axis',(0.,0.,-1.));
#13857=DIRECTION('',(1.,0.,0.));
#13858=DIRECTION('',(-1.,0.,0.));
#13859=DIRECTION('',(-1.,0.,0.));
#13860=DIRECTION('',(-1.,0.,0.));
#13861=DIRECTION('',(-1.,0.,0.));
#13862=DIRECTION('',(1.,0.,0.));
#13863=DIRECTION('',(1.,0.,0.));
#13864=DIRECTION('',(1.,0.,0.));
#13865=DIRECTION('center_axis',(0.500000000000017,-0.866025403784429,0.));
#13866=DIRECTION('ref_axis',(0.866025403784429,0.500000000000017,0.));
#13867=DIRECTION('',(0.,0.,1.));
#13868=DIRECTION('',(-0.866025403784429,-0.500000000000017,0.));
#13869=DIRECTION('',(0.,0.,-1.));
#13870=DIRECTION('center_axis',(1.,0.,0.));
#13871=DIRECTION('ref_axis',(0.,0.,-1.));
#13872=DIRECTION('center_axis',(-1.,0.,0.));
#13873=DIRECTION('ref_axis',(0.,0.,1.));
#13874=DIRECTION('',(0.,1.,0.));
#13875=DIRECTION('center_axis',(0.,0.,-1.));
#13876=DIRECTION('ref_axis',(-1.,0.,0.));
#13877=DIRECTION('',(0.,-1.,0.));
#13878=DIRECTION('',(0.,1.,0.));
#13879=DIRECTION('',(1.,0.,0.));
#13880=DIRECTION('',(0.,-1.,0.));
#13881=DIRECTION('',(-1.,0.,0.));
#13882=DIRECTION('center_axis',(1.,0.,0.));
#13883=DIRECTION('ref_axis',(0.,0.,-1.));
#13884=DIRECTION('center_axis',(-0.866025403784429,0.500000000000017,0.));
#13885=DIRECTION('ref_axis',(-0.500000000000017,-0.866025403784429,0.));
#13886=DIRECTION('',(0.,0.,-1.));
#13887=DIRECTION('center_axis',(-0.866025403784429,-0.500000000000017,0.));
#13888=DIRECTION('ref_axis',(0.500000000000017,-0.866025403784429,0.));
#13889=DIRECTION('center_axis',(-0.866025403784429,0.500000000000017,0.));
#13890=DIRECTION('ref_axis',(-0.500000000000017,-0.866025403784429,0.));
#13891=DIRECTION('',(0.,0.,-1.));
#13892=DIRECTION('center_axis',(-0.866025403784429,-0.500000000000017,0.));
#13893=DIRECTION('ref_axis',(0.500000000000017,-0.866025403784429,0.));
#13894=DIRECTION('center_axis',(0.866025403784429,-0.500000000000017,0.));
#13895=DIRECTION('ref_axis',(0.500000000000017,0.866025403784429,0.));
#13896=DIRECTION('center_axis',(0.866025403784429,0.500000000000017,0.));
#13897=DIRECTION('ref_axis',(-0.500000000000017,0.866025403784429,0.));
#13898=DIRECTION('',(0.,0.,-1.));
#13899=DIRECTION('center_axis',(0.866025403784429,-0.500000000000017,0.));
#13900=DIRECTION('ref_axis',(0.500000000000017,0.866025403784429,0.));
#13901=DIRECTION('center_axis',(-1.,0.,0.));
#13902=DIRECTION('ref_axis',(0.,0.,1.));
#13903=DIRECTION('',(0.,0.,-1.));
#13904=DIRECTION('center_axis',(-0.500000000000017,-0.866025403784429,0.));
#13905=DIRECTION('ref_axis',(0.866025403784429,-0.500000000000017,0.));
#13906=DIRECTION('',(-0.866025403784429,0.500000000000017,0.));
#13907=DIRECTION('',(0.,0.,-1.));
#13908=DIRECTION('center_axis',(0.500000000000017,-0.866025403784429,0.));
#13909=DIRECTION('ref_axis',(0.866025403784429,0.500000000000017,0.));
#13910=DIRECTION('',(-0.866025403784429,-0.500000000000017,0.));
#13911=DIRECTION('',(-0.866025403784429,-0.500000000000017,0.));
#13912=DIRECTION('center_axis',(0.866025403784429,-0.500000000000017,0.));
#13913=DIRECTION('ref_axis',(0.500000000000017,0.866025403784429,0.));
#13914=DIRECTION('',(0.,0.,-1.));
#13915=DIRECTION('center_axis',(0.866025403784429,0.500000000000017,0.));
#13916=DIRECTION('ref_axis',(-0.500000000000017,0.866025403784429,0.));
#13917=DIRECTION('center_axis',(0.866025403784429,-0.500000000000017,0.));
#13918=DIRECTION('ref_axis',(0.500000000000017,0.866025403784429,0.));
#13919=DIRECTION('',(0.,0.,-1.));
#13920=DIRECTION('center_axis',(0.866025403784429,0.500000000000017,0.));
#13921=DIRECTION('ref_axis',(-0.500000000000017,0.866025403784429,0.));
#13922=DIRECTION('center_axis',(-0.500000000000017,-0.866025403784429,0.));
#13923=DIRECTION('ref_axis',(0.866025403784429,-0.500000000000017,0.));
#13924=DIRECTION('',(-0.866025403784429,0.500000000000017,0.));
#13925=DIRECTION('',(-0.866025403784429,0.500000000000017,0.));
#13926=DIRECTION('center_axis',(1.,0.,0.));
#13927=DIRECTION('ref_axis',(0.,0.,-1.));
#13928=DIRECTION('',(0.,-1.,0.));
#13929=DIRECTION('center_axis',(0.,0.,1.));
#13930=DIRECTION('ref_axis',(1.,0.,0.));
#13931=DIRECTION('center_axis',(0.,0.,1.));
#13932=DIRECTION('ref_axis',(1.,0.,0.));
#13933=DIRECTION('center_axis',(0.,0.,1.));
#13934=DIRECTION('ref_axis',(1.,0.,0.));
#13935=DIRECTION('center_axis',(0.,0.,1.));
#13936=DIRECTION('ref_axis',(1.,0.,0.));
#13937=DIRECTION('center_axis',(0.,0.,1.));
#13938=DIRECTION('ref_axis',(1.,0.,0.));
#13939=DIRECTION('center_axis',(0.,0.,1.));
#13940=DIRECTION('ref_axis',(1.,0.,0.));
#13941=DIRECTION('center_axis',(0.,0.,1.));
#13942=DIRECTION('ref_axis',(1.,0.,0.));
#13943=DIRECTION('center_axis',(0.,0.,1.));
#13944=DIRECTION('ref_axis',(1.,0.,0.));
#13945=DIRECTION('center_axis',(0.,0.,1.));
#13946=DIRECTION('ref_axis',(1.,0.,0.));
#13947=DIRECTION('center_axis',(-0.866025403784429,-0.500000000000017,0.));
#13948=DIRECTION('ref_axis',(0.500000000000017,-0.866025403784429,0.));
#13949=DIRECTION('',(0.,0.,-1.));
#13950=DIRECTION('center_axis',(-0.866025403784429,0.500000000000017,0.));
#13951=DIRECTION('ref_axis',(-0.500000000000017,-0.866025403784429,0.));
#13952=DIRECTION('center_axis',(-0.866025403784429,-0.500000000000017,0.));
#13953=DIRECTION('ref_axis',(0.500000000000017,-0.866025403784429,0.));
#13954=DIRECTION('',(0.,0.,-1.));
#13955=DIRECTION('center_axis',(-0.866025403784429,0.500000000000017,0.));
#13956=DIRECTION('ref_axis',(-0.500000000000017,-0.866025403784429,0.));
#13957=DIRECTION('center_axis',(0.,0.,-1.));
#13958=DIRECTION('ref_axis',(-1.,0.,0.));
#13959=DIRECTION('',(0.,1.,0.));
#13960=DIRECTION('',(-1.,0.,0.));
#13961=DIRECTION('',(0.,1.,0.));
#13962=DIRECTION('',(1.,0.,0.));
#13963=DIRECTION('',(0.,-1.,0.));
#13964=DIRECTION('center_axis',(-1.,0.,0.));
#13965=DIRECTION('ref_axis',(0.,0.,1.));
#13966=DIRECTION('center_axis',(1.,0.,0.));
#13967=DIRECTION('ref_axis',(0.,0.,-1.));
#13968=DIRECTION('',(0.,0.,1.));
#13969=DIRECTION('center_axis',(0.500000000000017,0.866025403784429,0.));
#13970=DIRECTION('ref_axis',(-0.866025403784429,0.500000000000017,0.));
#13971=DIRECTION('',(0.,0.,1.));
#13972=DIRECTION('',(-0.866025403784429,0.500000000000017,0.));
#13973=DIRECTION('center_axis',(-0.500000000000017,0.866025403784429,0.));
#13974=DIRECTION('ref_axis',(-0.866025403784429,-0.500000000000017,0.));
#13975=DIRECTION('',(-0.866025403784429,-0.500000000000017,0.));
#13976=DIRECTION('',(-0.866025403784429,-0.500000000000017,0.));
#13977=DIRECTION('center_axis',(0.500000000000017,0.866025403784429,0.));
#13978=DIRECTION('ref_axis',(-0.866025403784429,0.500000000000017,0.));
#13979=DIRECTION('',(-0.866025403784429,0.500000000000017,0.));
#13980=DIRECTION('',(-0.866025403784429,0.500000000000017,0.));
#13981=DIRECTION('center_axis',(0.,0.,1.));
#13982=DIRECTION('ref_axis',(1.,0.,0.));
#13983=DIRECTION('center_axis',(0.,0.,1.));
#13984=DIRECTION('ref_axis',(1.,0.,0.));
#13985=DIRECTION('center_axis',(0.,0.,-1.));
#13986=DIRECTION('ref_axis',(-1.,0.,0.));
#13987=DIRECTION('center_axis',(0.,0.,-1.));
#13988=DIRECTION('ref_axis',(-1.,0.,0.));
#13989=DIRECTION('center_axis',(0.,0.,-1.));
#13990=DIRECTION('ref_axis',(-1.,0.,0.));
#13991=DIRECTION('center_axis',(0.,0.,-1.));
#13992=DIRECTION('ref_axis',(-1.,0.,0.));
#13993=DIRECTION('center_axis',(0.,1.,0.));
#13994=DIRECTION('ref_axis',(0.,0.,1.));
#13995=DIRECTION('',(1.,0.,0.));
#13996=DIRECTION('',(0.,0.,-1.));
#13997=DIRECTION('',(0.,0.,1.));
#13998=DIRECTION('center_axis',(1.,0.,0.));
#13999=DIRECTION('ref_axis',(0.,0.,-1.));
#14000=DIRECTION('',(0.,-1.,0.));
#14001=DIRECTION('',(0.,0.,-1.));
#14002=DIRECTION('center_axis',(0.,-1.,0.));
#14003=DIRECTION('ref_axis',(0.,0.,-1.));
#14004=DIRECTION('',(-1.,0.,0.));
#14005=DIRECTION('',(0.,0.,-1.));
#14006=DIRECTION('center_axis',(-1.,0.,0.));
#14007=DIRECTION('ref_axis',(0.,0.,1.));
#14008=DIRECTION('',(0.,1.,0.));
#14009=DIRECTION('center_axis',(-1.,0.,0.));
#14010=DIRECTION('ref_axis',(0.,0.,1.));
#14011=DIRECTION('',(0.,1.,0.));
#14012=DIRECTION('',(0.,0.,-1.));
#14013=DIRECTION('',(0.,0.,1.));
#14014=DIRECTION('center_axis',(0.,1.,0.));
#14015=DIRECTION('ref_axis',(0.,0.,1.));
#14016=DIRECTION('',(1.,0.,0.));
#14017=DIRECTION('',(0.,0.,-1.));
#14018=DIRECTION('center_axis',(1.,0.,0.));
#14019=DIRECTION('ref_axis',(0.,0.,-1.));
#14020=DIRECTION('',(0.,-1.,0.));
#14021=DIRECTION('',(0.,0.,-1.));
#14022=DIRECTION('center_axis',(0.,-1.,0.));
#14023=DIRECTION('ref_axis',(0.,0.,-1.));
#14024=DIRECTION('',(-1.,0.,0.));
#14025=DIRECTION('center_axis',(0.,0.,-1.));
#14026=DIRECTION('ref_axis',(-1.,0.,0.));
#14027=DIRECTION('center_axis',(0.,0.,1.));
#14028=DIRECTION('ref_axis',(1.,0.,0.));
#14029=DIRECTION('center_axis',(0.,0.,-1.));
#14030=DIRECTION('ref_axis',(-1.,0.,0.));
#14031=DIRECTION('center_axis',(0.,0.,1.));
#14032=DIRECTION('ref_axis',(1.,0.,0.));
#14033=DIRECTION('center_axis',(0.,0.,-1.));
#14034=DIRECTION('ref_axis',(-1.,0.,0.));
#14035=DIRECTION('center_axis',(0.,0.,-1.));
#14036=DIRECTION('ref_axis',(-1.,0.,0.));
#14037=DIRECTION('center_axis',(0.,0.,-1.));
#14038=DIRECTION('ref_axis',(-1.,0.,0.));
#14039=DIRECTION('center_axis',(0.,0.,-1.));
#14040=DIRECTION('ref_axis',(-1.,0.,0.));
#14041=DIRECTION('axis',(0.,0.,1.));
#14042=DIRECTION('refdir',(1.,0.,0.));
#14043=DIRECTION('center_axis',(0.,1.,0.));
#14044=DIRECTION('ref_axis',(0.,0.,1.));
#14045=DIRECTION('center_axis',(0.,1.,0.));
#14046=DIRECTION('ref_axis',(0.,0.,1.));
#14047=DIRECTION('',(0.,1.,0.));
#14048=DIRECTION('center_axis',(0.,1.,0.));
#14049=DIRECTION('ref_axis',(0.,0.,1.));
#14050=DIRECTION('center_axis',(0.,1.,0.));
#14051=DIRECTION('ref_axis',(0.,0.,1.));
#14052=DIRECTION('center_axis',(0.,1.,0.));
#14053=DIRECTION('ref_axis',(0.,0.,1.));
#14054=DIRECTION('',(0.,1.,0.));
#14055=DIRECTION('center_axis',(0.,1.,0.));
#14056=DIRECTION('ref_axis',(0.,0.,1.));
#14057=DIRECTION('center_axis',(0.,1.,0.));
#14058=DIRECTION('ref_axis',(0.,0.,1.));
#14059=DIRECTION('center_axis',(0.,1.,0.));
#14060=DIRECTION('ref_axis',(0.,0.,1.));
#14061=DIRECTION('',(0.,1.,0.));
#14062=DIRECTION('center_axis',(0.,1.,0.));
#14063=DIRECTION('ref_axis',(0.,0.,1.));
#14064=DIRECTION('center_axis',(0.,1.,0.));
#14065=DIRECTION('ref_axis',(0.,0.,1.));
#14066=DIRECTION('center_axis',(0.,1.,0.));
#14067=DIRECTION('ref_axis',(0.,0.,1.));
#14068=DIRECTION('',(0.,1.,0.));
#14069=DIRECTION('center_axis',(0.,1.,0.));
#14070=DIRECTION('ref_axis',(0.,0.,1.));
#14071=DIRECTION('center_axis',(0.,-1.,0.));
#14072=DIRECTION('ref_axis',(0.,0.,-1.));
#14073=DIRECTION('center_axis',(0.,1.,0.));
#14074=DIRECTION('ref_axis',(0.,0.,-1.));
#14075=DIRECTION('',(0.,-1.,0.));
#14076=DIRECTION('center_axis',(0.,1.,0.));
#14077=DIRECTION('ref_axis',(0.,0.,-1.));
#14078=DIRECTION('center_axis',(0.,-1.,0.));
#14079=DIRECTION('ref_axis',(0.,0.,-1.));
#14080=DIRECTION('center_axis',(0.,1.,0.));
#14081=DIRECTION('ref_axis',(0.,0.,-1.));
#14082=DIRECTION('',(0.,-1.,0.));
#14083=DIRECTION('center_axis',(0.,1.,0.));
#14084=DIRECTION('ref_axis',(0.,0.,-1.));
#14085=DIRECTION('center_axis',(0.,-1.,0.));
#14086=DIRECTION('ref_axis',(0.,0.,-1.));
#14087=DIRECTION('center_axis',(0.,1.,0.));
#14088=DIRECTION('ref_axis',(0.,0.,-1.));
#14089=DIRECTION('',(0.,-1.,0.));
#14090=DIRECTION('center_axis',(0.,1.,0.));
#14091=DIRECTION('ref_axis',(0.,0.,-1.));
#14092=DIRECTION('center_axis',(0.,-1.,0.));
#14093=DIRECTION('ref_axis',(0.,0.,-1.));
#14094=DIRECTION('center_axis',(0.,1.,0.));
#14095=DIRECTION('ref_axis',(0.,0.,-1.));
#14096=DIRECTION('',(0.,-1.,0.));
#14097=DIRECTION('center_axis',(0.,1.,0.));
#14098=DIRECTION('ref_axis',(0.,0.,-1.));
#14099=DIRECTION('center_axis',(0.,1.,0.));
#14100=DIRECTION('ref_axis',(0.,0.,1.));
#14101=DIRECTION('center_axis',(0.,1.,0.));
#14102=DIRECTION('ref_axis',(0.,0.,1.));
#14103=DIRECTION('',(0.,1.,0.));
#14104=DIRECTION('center_axis',(0.,1.,0.));
#14105=DIRECTION('ref_axis',(0.,0.,1.));
#14106=DIRECTION('center_axis',(0.,1.,0.));
#14107=DIRECTION('ref_axis',(0.,0.,1.));
#14108=DIRECTION('center_axis',(0.,1.,0.));
#14109=DIRECTION('ref_axis',(0.,0.,1.));
#14110=DIRECTION('',(0.,1.,0.));
#14111=DIRECTION('center_axis',(0.,1.,0.));
#14112=DIRECTION('ref_axis',(0.,0.,1.));
#14113=DIRECTION('center_axis',(0.,1.,0.));
#14114=DIRECTION('ref_axis',(0.,0.,1.));
#14115=DIRECTION('center_axis',(0.,1.,0.));
#14116=DIRECTION('ref_axis',(0.,0.,1.));
#14117=DIRECTION('',(0.,1.,0.));
#14118=DIRECTION('center_axis',(0.,1.,0.));
#14119=DIRECTION('ref_axis',(0.,0.,1.));
#14120=DIRECTION('center_axis',(0.,1.,0.));
#14121=DIRECTION('ref_axis',(0.,0.,1.));
#14122=DIRECTION('center_axis',(0.,1.,0.));
#14123=DIRECTION('ref_axis',(0.,0.,1.));
#14124=DIRECTION('',(0.,1.,0.));
#14125=DIRECTION('center_axis',(0.,1.,0.));
#14126=DIRECTION('ref_axis',(0.,0.,1.));
#14127=DIRECTION('center_axis',(0.,-1.,0.));
#14128=DIRECTION('ref_axis',(0.,0.,-1.));
#14129=DIRECTION('center_axis',(0.,1.,0.));
#14130=DIRECTION('ref_axis',(0.,0.,-1.));
#14131=DIRECTION('',(0.,-1.,0.));
#14132=DIRECTION('center_axis',(0.,1.,0.));
#14133=DIRECTION('ref_axis',(0.,0.,-1.));
#14134=DIRECTION('center_axis',(0.,-1.,0.));
#14135=DIRECTION('ref_axis',(0.,0.,-1.));
#14136=DIRECTION('center_axis',(0.,1.,0.));
#14137=DIRECTION('ref_axis',(0.,0.,-1.));
#14138=DIRECTION('',(0.,-1.,0.));
#14139=DIRECTION('center_axis',(0.,1.,0.));
#14140=DIRECTION('ref_axis',(0.,0.,-1.));
#14141=DIRECTION('center_axis',(0.,-1.,0.));
#14142=DIRECTION('ref_axis',(0.,0.,-1.));
#14143=DIRECTION('center_axis',(0.,1.,0.));
#14144=DIRECTION('ref_axis',(0.,0.,-1.));
#14145=DIRECTION('',(0.,-1.,0.));
#14146=DIRECTION('center_axis',(0.,1.,0.));
#14147=DIRECTION('ref_axis',(0.,0.,-1.));
#14148=DIRECTION('center_axis',(0.,-1.,0.));
#14149=DIRECTION('ref_axis',(0.,0.,-1.));
#14150=DIRECTION('center_axis',(0.,1.,0.));
#14151=DIRECTION('ref_axis',(0.,0.,-1.));
#14152=DIRECTION('',(0.,-1.,0.));
#14153=DIRECTION('center_axis',(0.,1.,0.));
#14154=DIRECTION('ref_axis',(0.,0.,-1.));
#14155=DIRECTION('center_axis',(0.,-1.,0.));
#14156=DIRECTION('ref_axis',(0.,0.,-1.));
#14157=DIRECTION('center_axis',(0.,1.,0.));
#14158=DIRECTION('ref_axis',(0.,0.,-1.));
#14159=DIRECTION('',(0.,-1.,0.));
#14160=DIRECTION('center_axis',(0.,1.,0.));
#14161=DIRECTION('ref_axis',(0.,0.,-1.));
#14162=DIRECTION('center_axis',(0.,-1.,0.));
#14163=DIRECTION('ref_axis',(0.,0.,-1.));
#14164=DIRECTION('center_axis',(0.,1.,0.));
#14165=DIRECTION('ref_axis',(0.,0.,-1.));
#14166=DIRECTION('',(0.,-1.,0.));
#14167=DIRECTION('center_axis',(0.,1.,0.));
#14168=DIRECTION('ref_axis',(0.,0.,-1.));
#14169=DIRECTION('center_axis',(0.,-1.,0.));
#14170=DIRECTION('ref_axis',(0.,0.,-1.));
#14171=DIRECTION('center_axis',(0.,1.,0.));
#14172=DIRECTION('ref_axis',(0.,0.,-1.));
#14173=DIRECTION('',(0.,-1.,0.));
#14174=DIRECTION('center_axis',(0.,1.,0.));
#14175=DIRECTION('ref_axis',(0.,0.,-1.));
#14176=DIRECTION('center_axis',(0.,-1.,0.));
#14177=DIRECTION('ref_axis',(0.,0.,-1.));
#14178=DIRECTION('center_axis',(0.,1.,0.));
#14179=DIRECTION('ref_axis',(0.,0.,-1.));
#14180=DIRECTION('',(0.,-1.,0.));
#14181=DIRECTION('center_axis',(0.,1.,0.));
#14182=DIRECTION('ref_axis',(0.,0.,-1.));
#14183=DIRECTION('center_axis',(0.,-1.,0.));
#14184=DIRECTION('ref_axis',(0.,0.,-1.));
#14185=DIRECTION('center_axis',(0.,1.,0.));
#14186=DIRECTION('ref_axis',(0.,0.,-1.));
#14187=DIRECTION('',(0.,-1.,0.));
#14188=DIRECTION('center_axis',(0.,1.,0.));
#14189=DIRECTION('ref_axis',(0.,0.,-1.));
#14190=DIRECTION('center_axis',(0.,-1.,0.));
#14191=DIRECTION('ref_axis',(0.,0.,-1.));
#14192=DIRECTION('center_axis',(0.,1.,0.));
#14193=DIRECTION('ref_axis',(0.,0.,-1.));
#14194=DIRECTION('',(0.,-1.,0.));
#14195=DIRECTION('center_axis',(0.,1.,0.));
#14196=DIRECTION('ref_axis',(0.,0.,-1.));
#14197=DIRECTION('center_axis',(0.,-1.,0.));
#14198=DIRECTION('ref_axis',(0.,0.,-1.));
#14199=DIRECTION('center_axis',(0.,1.,0.));
#14200=DIRECTION('ref_axis',(0.,0.,-1.));
#14201=DIRECTION('',(0.,-1.,0.));
#14202=DIRECTION('center_axis',(0.,1.,0.));
#14203=DIRECTION('ref_axis',(0.,0.,-1.));
#14204=DIRECTION('center_axis',(0.,-1.,0.));
#14205=DIRECTION('ref_axis',(0.,0.,-1.));
#14206=DIRECTION('center_axis',(0.,1.,0.));
#14207=DIRECTION('ref_axis',(0.,0.,-1.));
#14208=DIRECTION('',(0.,-1.,0.));
#14209=DIRECTION('center_axis',(0.,1.,0.));
#14210=DIRECTION('ref_axis',(0.,0.,-1.));
#14211=DIRECTION('center_axis',(0.,-1.,0.));
#14212=DIRECTION('ref_axis',(0.,0.,-1.));
#14213=DIRECTION('center_axis',(0.,1.,0.));
#14214=DIRECTION('ref_axis',(0.,0.,-1.));
#14215=DIRECTION('',(0.,-1.,0.));
#14216=DIRECTION('center_axis',(0.,1.,0.));
#14217=DIRECTION('ref_axis',(0.,0.,-1.));
#14218=DIRECTION('center_axis',(0.,-1.,0.));
#14219=DIRECTION('ref_axis',(0.,0.,-1.));
#14220=DIRECTION('',(-8.65956056235493E-17,-0.707106781186548,0.707106781186547));
#14221=DIRECTION('center_axis',(0.,1.,0.));
#14222=DIRECTION('ref_axis',(0.,0.,-1.));
#14223=DIRECTION('center_axis',(0.,-1.,0.));
#14224=DIRECTION('ref_axis',(0.,0.,-1.));
#14225=DIRECTION('',(-8.65956056235493E-17,-0.707106781186548,0.707106781186547));
#14226=DIRECTION('center_axis',(0.,1.,0.));
#14227=DIRECTION('ref_axis',(0.,0.,-1.));
#14228=DIRECTION('center_axis',(0.,-1.,0.));
#14229=DIRECTION('ref_axis',(0.,0.,-1.));
#14230=DIRECTION('',(-8.65956056235493E-17,-0.707106781186548,0.707106781186547));
#14231=DIRECTION('center_axis',(0.,1.,0.));
#14232=DIRECTION('ref_axis',(0.,0.,-1.));
#14233=DIRECTION('center_axis',(0.,-1.,0.));
#14234=DIRECTION('ref_axis',(0.,0.,-1.));
#14235=DIRECTION('',(-8.65956056235493E-17,-0.707106781186548,0.707106781186547));
#14236=DIRECTION('center_axis',(0.,1.,0.));
#14237=DIRECTION('ref_axis',(0.,0.,-1.));
#14238=DIRECTION('center_axis',(0.,-1.,0.));
#14239=DIRECTION('ref_axis',(0.,0.,-1.));
#14240=DIRECTION('',(-8.65956056235493E-17,-0.707106781186547,0.707106781186547));
#14241=DIRECTION('center_axis',(0.,1.,0.));
#14242=DIRECTION('ref_axis',(0.,0.,-1.));
#14243=DIRECTION('center_axis',(0.,-1.,0.));
#14244=DIRECTION('ref_axis',(0.,0.,-1.));
#14245=DIRECTION('',(-8.65956056235493E-17,-0.707106781186547,0.707106781186547));
#14246=DIRECTION('center_axis',(0.,1.,0.));
#14247=DIRECTION('ref_axis',(0.,0.,-1.));
#14248=DIRECTION('center_axis',(0.,-1.,0.));
#14249=DIRECTION('ref_axis',(0.,0.,-1.));
#14250=DIRECTION('',(-8.65956056235493E-17,-0.707106781186547,0.707106781186547));
#14251=DIRECTION('center_axis',(0.,1.,0.));
#14252=DIRECTION('ref_axis',(0.,0.,-1.));
#14253=DIRECTION('center_axis',(0.,-1.,0.));
#14254=DIRECTION('ref_axis',(0.,0.,-1.));
#14255=DIRECTION('',(-8.65956056235493E-17,-0.707106781186548,0.707106781186547));
#14256=DIRECTION('center_axis',(0.,1.,0.));
#14257=DIRECTION('ref_axis',(0.,0.,-1.));
#14258=DIRECTION('center_axis',(0.,-1.,0.));
#14259=DIRECTION('ref_axis',(0.,0.,-1.));
#14260=DIRECTION('',(-8.65951884466615E-17,-0.707110187677941,0.707103374678744));
#14261=DIRECTION('center_axis',(0.,1.,0.));
#14262=DIRECTION('ref_axis',(0.,0.,-1.));
#14263=DIRECTION('center_axis',(0.,0.,-1.));
#14264=DIRECTION('ref_axis',(-1.,0.,0.));
#14265=DIRECTION('center_axis',(0.,0.,-1.));
#14266=DIRECTION('ref_axis',(-1.,0.,0.));
#14267=DIRECTION('',(0.,0.,-1.));
#14268=DIRECTION('center_axis',(0.,0.,-1.));
#14269=DIRECTION('ref_axis',(-1.,0.,0.));
#14270=DIRECTION('center_axis',(0.,0.,-1.));
#14271=DIRECTION('ref_axis',(-1.,0.,0.));
#14272=DIRECTION('center_axis',(0.,0.,-1.));
#14273=DIRECTION('ref_axis',(-1.,0.,0.));
#14274=DIRECTION('',(0.,0.,-1.));
#14275=DIRECTION('center_axis',(0.,0.,-1.));
#14276=DIRECTION('ref_axis',(-1.,0.,0.));
#14277=DIRECTION('center_axis',(0.,0.,-1.));
#14278=DIRECTION('ref_axis',(-1.,0.,0.));
#14279=DIRECTION('center_axis',(0.,0.,-1.));
#14280=DIRECTION('ref_axis',(-1.,0.,0.));
#14281=DIRECTION('',(0.,0.,-1.));
#14282=DIRECTION('center_axis',(0.,0.,-1.));
#14283=DIRECTION('ref_axis',(-1.,0.,0.));
#14284=DIRECTION('center_axis',(0.,0.,-1.));
#14285=DIRECTION('ref_axis',(-1.,0.,0.));
#14286=DIRECTION('center_axis',(0.,0.,-1.));
#14287=DIRECTION('ref_axis',(-1.,0.,0.));
#14288=DIRECTION('',(0.,0.,-1.));
#14289=DIRECTION('center_axis',(0.,0.,-1.));
#14290=DIRECTION('ref_axis',(-1.,0.,0.));
#14291=DIRECTION('center_axis',(0.,0.,-1.));
#14292=DIRECTION('ref_axis',(-1.,0.,0.));
#14293=DIRECTION('center_axis',(0.,0.,1.));
#14294=DIRECTION('ref_axis',(-1.,0.,0.));
#14295=DIRECTION('',(0.,0.,-1.));
#14296=DIRECTION('center_axis',(0.,0.,1.));
#14297=DIRECTION('ref_axis',(-1.,0.,0.));
#14298=DIRECTION('center_axis',(0.,0.,-1.));
#14299=DIRECTION('ref_axis',(-1.,0.,0.));
#14300=DIRECTION('center_axis',(0.,0.,1.));
#14301=DIRECTION('ref_axis',(-1.,0.,0.));
#14302=DIRECTION('',(0.,0.,-1.));
#14303=DIRECTION('center_axis',(0.,0.,1.));
#14304=DIRECTION('ref_axis',(-1.,0.,0.));
#14305=DIRECTION('center_axis',(0.,0.,-1.));
#14306=DIRECTION('ref_axis',(-1.,0.,0.));
#14307=DIRECTION('center_axis',(0.,0.,1.));
#14308=DIRECTION('ref_axis',(-1.,0.,0.));
#14309=DIRECTION('',(0.,0.,-1.));
#14310=DIRECTION('center_axis',(0.,0.,1.));
#14311=DIRECTION('ref_axis',(-1.,0.,0.));
#14312=DIRECTION('center_axis',(0.,0.,-1.));
#14313=DIRECTION('ref_axis',(-1.,0.,0.));
#14314=DIRECTION('center_axis',(0.,0.,1.));
#14315=DIRECTION('ref_axis',(-1.,0.,0.));
#14316=DIRECTION('',(0.,0.,-1.));
#14317=DIRECTION('center_axis',(0.,0.,1.));
#14318=DIRECTION('ref_axis',(-1.,0.,0.));
#14319=DIRECTION('center_axis',(0.,-1.,0.));
#14320=DIRECTION('ref_axis',(0.,0.,-1.));
#14321=DIRECTION('',(0.,0.,1.));
#14322=DIRECTION('',(1.,0.,0.));
#14323=DIRECTION('center_axis',(0.,1.,0.));
#14324=DIRECTION('ref_axis',(1.73472347597681E-15,0.,-1.));
#14325=DIRECTION('',(0.,0.,-1.));
#14326=DIRECTION('center_axis',(0.,1.,0.));
#14327=DIRECTION('ref_axis',(0.,0.,-1.));
#14328=DIRECTION('',(-1.,0.,0.));
#14329=DIRECTION('center_axis',(1.,0.,0.));
#14330=DIRECTION('ref_axis',(0.,0.,-1.));
#14331=DIRECTION('center_axis',(1.,0.,0.));
#14332=DIRECTION('ref_axis',(0.,0.,-1.));
#14333=DIRECTION('center_axis',(-0.246140467955622,-0.968967287951173,-0.0227434587329154));
#14334=DIRECTION('ref_axis',(0.96923416677013,-0.246072692904075,-0.00577579192399951));
#14335=DIRECTION('',(-1.,0.,0.));
#14336=DIRECTION('center_axis',(-1.,0.,0.));
#14337=DIRECTION('ref_axis',(0.,0.,1.));
#14338=DIRECTION('',(0.,1.,0.));
#14339=DIRECTION('',(0.,0.,-1.));
#14340=DIRECTION('',(0.,1.,0.));
#14341=DIRECTION('center_axis',(-1.,0.,0.));
#14342=DIRECTION('ref_axis',(0.,0.,-1.));
#14343=DIRECTION('',(0.,0.,1.));
#14344=DIRECTION('center_axis',(-1.,0.,0.));
#14345=DIRECTION('ref_axis',(0.,0.,-1.));
#14346=DIRECTION('',(0.,-1.,0.));
#14347=DIRECTION('',(0.,0.,-1.));
#14348=DIRECTION('',(0.,-1.,0.));
#14349=DIRECTION('center_axis',(-1.,0.,0.));
#14350=DIRECTION('ref_axis',(0.,0.,-1.));
#14351=DIRECTION('center_axis',(1.,0.,0.));
#14352=DIRECTION('ref_axis',(0.,0.,-1.));
#14353=DIRECTION('',(1.,0.,0.));
#14354=DIRECTION('center_axis',(0.246140467946646,0.968967287891977,-0.0227434613520755));
#14355=DIRECTION('ref_axis',(0.969234166772409,-0.246072692990846,0.0057757878446833));
#14356=DIRECTION('center_axis',(0.,-1.,0.));
#14357=DIRECTION('ref_axis',(0.,0.,-1.));
#14358=DIRECTION('',(0.,1.,0.));
#14359=DIRECTION('',(0.,1.,0.));
#14360=DIRECTION('center_axis',(0.,1.,0.));
#14361=DIRECTION('ref_axis',(-1.15648231731787E-15,0.,-1.));
#14362=DIRECTION('',(0.,-1.,0.));
#14363=DIRECTION('center_axis',(-1.,0.,0.));
#14364=DIRECTION('ref_axis',(0.,0.,1.));
#14365=DIRECTION('',(0.,0.,1.));
#14366=DIRECTION('',(0.,1.,0.));
#14367=DIRECTION('center_axis',(0.,-1.,0.));
#14368=DIRECTION('ref_axis',(0.,0.,-1.));
#14369=DIRECTION('center_axis',(0.,1.,0.));
#14370=DIRECTION('ref_axis',(0.,0.,-1.));
#14371=DIRECTION('',(0.,-1.,0.));
#14372=DIRECTION('',(0.,-1.,0.));
#14373=DIRECTION('center_axis',(0.,-1.,0.));
#14374=DIRECTION('ref_axis',(0.,0.,-1.));
#14375=DIRECTION('',(-1.,0.,0.));
#14376=DIRECTION('',(1.,0.,0.));
#14377=DIRECTION('center_axis',(0.,0.,1.));
#14378=DIRECTION('ref_axis',(1.,0.,0.));
#14379=DIRECTION('',(0.866025403784817,-0.499999999999345,0.));
#14380=DIRECTION('center_axis',(0.,0.,1.));
#14381=DIRECTION('ref_axis',(1.,0.,0.));
#14382=DIRECTION('',(0.,-1.,0.));
#14383=DIRECTION('center_axis',(0.,0.,1.));
#14384=DIRECTION('ref_axis',(1.,0.,0.));
#14385=DIRECTION('',(-1.,0.,0.));
#14386=DIRECTION('center_axis',(0.,0.,1.));
#14387=DIRECTION('ref_axis',(1.,0.,0.));
#14388=DIRECTION('',(0.,-0.0469178636304674,0.998898750661123));
#14389=DIRECTION('',(0.,0.046917863628385,0.998898750661221));
#14390=DIRECTION('center_axis',(0.,0.,-1.));
#14391=DIRECTION('ref_axis',(-1.,0.,0.));
#14392=DIRECTION('center_axis',(0.,0.,-1.));
#14393=DIRECTION('ref_axis',(-1.,0.,0.));
#14394=DIRECTION('',(0.,1.,0.));
#14395=DIRECTION('center_axis',(0.,0.,-1.));
#14396=DIRECTION('ref_axis',(-1.,0.,0.));
#14397=DIRECTION('',(-0.866025403784817,0.499999999999345,0.));
#14398=DIRECTION('center_axis',(0.,0.,-1.));
#14399=DIRECTION('ref_axis',(-1.,0.,0.));
#14400=DIRECTION('',(1.,0.,0.));
#14401=DIRECTION('center_axis',(1.,0.,0.));
#14402=DIRECTION('ref_axis',(0.,0.,-1.));
#14403=DIRECTION('',(-1.,0.,0.));
#14404=DIRECTION('center_axis',(0.785618915719221,0.618540328946539,0.0145182895295127));
#14405=DIRECTION('ref_axis',(0.0114064440257488,-0.0379409523114369,0.999214880379785));
#14406=DIRECTION('center_axis',(1.,0.,0.));
#14407=DIRECTION('ref_axis',(0.,0.,-1.));
#14408=DIRECTION('center_axis',(0.785618915707418,0.618540328961463,-0.0145182895323779));
#14409=DIRECTION('ref_axis',(-0.0114064440275411,-0.00898185763283676,-0.999894604079905));
#14410=DIRECTION('',(1.,0.,0.));
#14411=DIRECTION('center_axis',(-0.500000000000017,-0.866025403784429,0.));
#14412=DIRECTION('ref_axis',(0.866025403784429,-0.500000000000017,0.));
#14413=DIRECTION('',(-0.866025403784429,0.500000000000017,0.));
#14414=DIRECTION('',(0.,0.,-1.));
#14415=DIRECTION('',(0.,0.,1.));
#14416=DIRECTION('',(0.,0.,1.));
#14417=DIRECTION('center_axis',(0.,0.,1.));
#14418=DIRECTION('ref_axis',(1.,0.,0.));
#14419=DIRECTION('center_axis',(0.,0.,-1.));
#14420=DIRECTION('ref_axis',(1.,1.73472347597681E-15,0.));
#14421=DIRECTION('',(0.,0.,-1.));
#14422=DIRECTION('center_axis',(0.,0.,1.));
#14423=DIRECTION('ref_axis',(1.,0.,0.));
#14424=DIRECTION('',(0.,0.,1.));
#14425=DIRECTION('center_axis',(0.,0.,-1.));
#14426=DIRECTION('ref_axis',(1.,0.,0.));
#14427=DIRECTION('',(0.,0.,-1.));
#14428=DIRECTION('center_axis',(0.,1.,0.));
#14429=DIRECTION('ref_axis',(0.,0.,1.));
#14430=DIRECTION('',(1.,0.,0.));
#14431=DIRECTION('',(0.,0.,-1.));
#14432=DIRECTION('center_axis',(0.,0.,1.));
#14433=DIRECTION('ref_axis',(1.,0.,0.));
#14434=DIRECTION('center_axis',(0.,0.,-1.));
#14435=DIRECTION('ref_axis',(1.,0.,0.));
#14436=DIRECTION('',(0.,-1.85865077509542E-12,-1.));
#14437=DIRECTION('',(0.,-1.85865077509542E-12,-1.));
#14438=DIRECTION('center_axis',(0.,-1.,0.));
#14439=DIRECTION('ref_axis',(0.,0.,-1.));
#14440=DIRECTION('',(0.,0.,-1.));
#14441=DIRECTION('',(0.,0.,1.));
#14442=DIRECTION('',(1.,0.,0.));
#14443=DIRECTION('center_axis',(0.,0.,-1.));
#14444=DIRECTION('ref_axis',(-1.,0.,0.));
#14445=DIRECTION('center_axis',(0.,0.,1.));
#14446=DIRECTION('ref_axis',(-1.,0.,0.));
#14447=DIRECTION('',(0.,0.,1.));
#14448=DIRECTION('center_axis',(0.,0.,-1.));
#14449=DIRECTION('ref_axis',(-1.,0.,0.));
#14450=DIRECTION('',(0.,0.,-1.));
#14451=DIRECTION('center_axis',(0.,0.,1.));
#14452=DIRECTION('ref_axis',(-1.,0.,0.));
#14453=DIRECTION('',(0.,0.,1.));
#14454=DIRECTION('center_axis',(-0.500000000000017,-0.866025403784429,0.));
#14455=DIRECTION('ref_axis',(0.866025403784429,-0.500000000000017,0.));
#14456=DIRECTION('',(0.866025403784429,-0.500000000000017,0.));
#14457=DIRECTION('center_axis',(0.,0.,-1.));
#14458=DIRECTION('ref_axis',(-1.,0.,0.));
#14459=DIRECTION('center_axis',(0.,0.,1.));
#14460=DIRECTION('ref_axis',(-1.,0.,0.));
#14461=DIRECTION('center_axis',(0.,0.,1.));
#14462=DIRECTION('ref_axis',(1.,0.,0.));
#14463=DIRECTION('',(0.,-1.,0.));
#14464=DIRECTION('center_axis',(0.,0.,-1.));
#14465=DIRECTION('ref_axis',(-1.,0.,0.));
#14466=DIRECTION('',(0.,1.,0.));
#14467=DIRECTION('center_axis',(-1.,0.,0.));
#14468=DIRECTION('ref_axis',(0.,0.,1.));
#14469=DIRECTION('center_axis',(-1.,0.,0.));
#14470=DIRECTION('ref_axis',(0.,0.,1.));
#14471=DIRECTION('center_axis',(0.,-1.,0.));
#14472=DIRECTION('ref_axis',(0.,0.,-1.));
#14473=DIRECTION('center_axis',(0.,1.,0.));
#14474=DIRECTION('ref_axis',(0.,0.,-1.));
#14475=DIRECTION('',(0.,1.,0.));
#14476=DIRECTION('center_axis',(0.,-1.,0.));
#14477=DIRECTION('ref_axis',(0.,0.,-1.));
#14478=DIRECTION('center_axis',(0.,-1.,0.));
#14479=DIRECTION('ref_axis',(0.,0.,-1.));
#14480=DIRECTION('center_axis',(0.,1.,0.));
#14481=DIRECTION('ref_axis',(0.,0.,-1.));
#14482=DIRECTION('',(0.,1.,0.));
#14483=DIRECTION('center_axis',(0.,-1.,0.));
#14484=DIRECTION('ref_axis',(0.,0.,-1.));
#14485=DIRECTION('center_axis',(0.,-1.,0.));
#14486=DIRECTION('ref_axis',(0.,0.,-1.));
#14487=DIRECTION('center_axis',(0.,1.,0.));
#14488=DIRECTION('ref_axis',(0.,0.,-1.));
#14489=DIRECTION('',(0.,1.,0.));
#14490=DIRECTION('center_axis',(0.,-1.,0.));
#14491=DIRECTION('ref_axis',(0.,0.,-1.));
#14492=DIRECTION('center_axis',(0.,-1.,0.));
#14493=DIRECTION('ref_axis',(0.,0.,-1.));
#14494=DIRECTION('center_axis',(0.,1.,0.));
#14495=DIRECTION('ref_axis',(0.,0.,-1.));
#14496=DIRECTION('',(0.,1.,0.));
#14497=DIRECTION('center_axis',(0.,-1.,0.));
#14498=DIRECTION('ref_axis',(0.,0.,-1.));
#14499=DIRECTION('center_axis',(0.,-1.,0.));
#14500=DIRECTION('ref_axis',(0.,0.,-1.));
#14501=DIRECTION('center_axis',(0.,1.,0.));
#14502=DIRECTION('ref_axis',(0.,0.,-1.));
#14503=DIRECTION('',(0.,1.,0.));
#14504=DIRECTION('center_axis',(0.,-1.,0.));
#14505=DIRECTION('ref_axis',(0.,0.,-1.));
#14506=DIRECTION('center_axis',(0.,-1.,0.));
#14507=DIRECTION('ref_axis',(0.,0.,-1.));
#14508=DIRECTION('center_axis',(0.,1.,0.));
#14509=DIRECTION('ref_axis',(0.,0.,-1.));
#14510=DIRECTION('',(0.,1.,0.));
#14511=DIRECTION('center_axis',(0.,-1.,0.));
#14512=DIRECTION('ref_axis',(0.,0.,-1.));
#14513=DIRECTION('center_axis',(0.,-1.,0.));
#14514=DIRECTION('ref_axis',(0.,0.,-1.));
#14515=DIRECTION('center_axis',(0.,1.,0.));
#14516=DIRECTION('ref_axis',(0.,0.,-1.));
#14517=DIRECTION('',(0.,1.,0.));
#14518=DIRECTION('center_axis',(0.,-1.,0.));
#14519=DIRECTION('ref_axis',(0.,0.,-1.));
#14520=DIRECTION('center_axis',(0.,-1.,0.));
#14521=DIRECTION('ref_axis',(0.,0.,-1.));
#14522=DIRECTION('center_axis',(0.,1.,0.));
#14523=DIRECTION('ref_axis',(0.,0.,-1.));
#14524=DIRECTION('',(0.,1.,0.));
#14525=DIRECTION('center_axis',(0.,-1.,0.));
#14526=DIRECTION('ref_axis',(0.,0.,-1.));
#14527=DIRECTION('axis',(0.,0.,1.));
#14528=DIRECTION('refdir',(1.,0.,0.));
#14529=DIRECTION('center_axis',(0.,1.,0.));
#14530=DIRECTION('ref_axis',(0.,0.,1.));
#14531=DIRECTION('center_axis',(0.,-1.,0.));
#14532=DIRECTION('ref_axis',(0.,0.,1.));
#14533=DIRECTION('',(-8.65956056235494E-17,0.707106781186547,-0.707106781186548));
#14534=DIRECTION('center_axis',(0.,1.,0.));
#14535=DIRECTION('ref_axis',(0.,0.,1.));
#14536=DIRECTION('center_axis',(0.,-1.,0.));
#14537=DIRECTION('ref_axis',(0.,0.,1.));
#14538=DIRECTION('center_axis',(0.,1.,0.));
#14539=DIRECTION('ref_axis',(0.,0.,1.));
#14540=DIRECTION('center_axis',(0.,1.,0.));
#14541=DIRECTION('ref_axis',(0.,0.,1.));
#14542=DIRECTION('',(0.,1.,0.));
#14543=DIRECTION('center_axis',(0.,1.,0.));
#14544=DIRECTION('ref_axis',(0.,0.,1.));
#14545=DIRECTION('center_axis',(0.,1.,0.));
#14546=DIRECTION('ref_axis',(0.,0.,1.));
#14547=DIRECTION('center_axis',(0.,1.,0.));
#14548=DIRECTION('ref_axis',(0.,0.,1.));
#14549=DIRECTION('',(0.,1.,0.));
#14550=DIRECTION('center_axis',(0.,1.,0.));
#14551=DIRECTION('ref_axis',(0.,0.,1.));
#14552=DIRECTION('center_axis',(0.,1.,0.));
#14553=DIRECTION('ref_axis',(0.,0.,1.));
#14554=DIRECTION('center_axis',(0.,1.,0.));
#14555=DIRECTION('ref_axis',(0.,0.,1.));
#14556=DIRECTION('',(0.,1.,0.));
#14557=DIRECTION('center_axis',(0.,1.,0.));
#14558=DIRECTION('ref_axis',(0.,0.,1.));
#14559=DIRECTION('center_axis',(0.,1.,0.));
#14560=DIRECTION('ref_axis',(0.,0.,1.));
#14561=DIRECTION('center_axis',(0.,1.,0.));
#14562=DIRECTION('ref_axis',(0.,0.,1.));
#14563=DIRECTION('',(0.,1.,0.));
#14564=DIRECTION('center_axis',(0.,1.,0.));
#14565=DIRECTION('ref_axis',(0.,0.,1.));
#14566=DIRECTION('center_axis',(0.,1.,0.));
#14567=DIRECTION('ref_axis',(0.,0.,1.));
#14568=DIRECTION('center_axis',(0.,1.,0.));
#14569=DIRECTION('ref_axis',(0.,0.,1.));
#14570=DIRECTION('',(0.,1.,0.));
#14571=DIRECTION('center_axis',(0.,1.,0.));
#14572=DIRECTION('ref_axis',(0.,0.,1.));
#14573=DIRECTION('center_axis',(0.,1.,0.));
#14574=DIRECTION('ref_axis',(0.,0.,1.));
#14575=DIRECTION('center_axis',(0.,1.,0.));
#14576=DIRECTION('ref_axis',(0.,0.,1.));
#14577=DIRECTION('',(0.,1.,0.));
#14578=DIRECTION('center_axis',(0.,1.,0.));
#14579=DIRECTION('ref_axis',(0.,0.,1.));
#14580=DIRECTION('center_axis',(0.,1.,0.));
#14581=DIRECTION('ref_axis',(0.,0.,1.));
#14582=DIRECTION('center_axis',(0.,1.,0.));
#14583=DIRECTION('ref_axis',(0.,0.,1.));
#14584=DIRECTION('',(0.,1.,0.));
#14585=DIRECTION('center_axis',(0.,1.,0.));
#14586=DIRECTION('ref_axis',(0.,0.,1.));
#14587=DIRECTION('center_axis',(0.,1.,0.));
#14588=DIRECTION('ref_axis',(0.,0.,1.));
#14589=DIRECTION('center_axis',(0.,1.,0.));
#14590=DIRECTION('ref_axis',(0.,0.,1.));
#14591=DIRECTION('',(0.,1.,0.));
#14592=DIRECTION('center_axis',(0.,1.,0.));
#14593=DIRECTION('ref_axis',(0.,0.,1.));
#14594=DIRECTION('center_axis',(0.,-1.,0.));
#14595=DIRECTION('ref_axis',(0.,0.,-1.));
#14596=DIRECTION('center_axis',(0.,1.,0.));
#14597=DIRECTION('ref_axis',(0.,0.,1.));
#14598=DIRECTION('',(0.,-1.,0.));
#14599=DIRECTION('center_axis',(0.,1.,0.));
#14600=DIRECTION('ref_axis',(0.,0.,1.));
#14601=DIRECTION('center_axis',(0.,-1.,0.));
#14602=DIRECTION('ref_axis',(0.,0.,-1.));
#14603=DIRECTION('',(0.,-1.,0.));
#14604=DIRECTION('center_axis',(0.,1.,0.));
#14605=DIRECTION('ref_axis',(0.,0.,1.));
#14606=DIRECTION('center_axis',(0.,1.,0.));
#14607=DIRECTION('ref_axis',(0.,0.,1.));
#14608=DIRECTION('',(0.122369609545525,0.,-0.992484598701499));
#14609=DIRECTION('center_axis',(0.,1.,0.));
#14610=DIRECTION('ref_axis',(0.,0.,1.));
#14611=DIRECTION('',(-0.122369609545525,0.,-0.992484598701499));
#14612=DIRECTION('center_axis',(0.,1.,0.));
#14613=DIRECTION('ref_axis',(0.,0.,1.));
#14614=DIRECTION('center_axis',(0.,1.,0.));
#14615=DIRECTION('ref_axis',(0.,0.,1.));
#14616=DIRECTION('center_axis',(0.,1.,0.));
#14617=DIRECTION('ref_axis',(0.,0.,1.));
#14618=DIRECTION('',(0.122369609545525,0.,-0.992484598701499));
#14619=DIRECTION('center_axis',(0.,1.,0.));
#14620=DIRECTION('ref_axis',(0.,0.,1.));
#14621=DIRECTION('',(-0.122369609545525,0.,-0.992484598701499));
#14622=DIRECTION('center_axis',(0.,-1.,0.));
#14623=DIRECTION('ref_axis',(1.22464679914735E-16,0.,1.));
#14624=DIRECTION('',(0.,-1.,0.));
#14625=DIRECTION('',(0.,-1.,0.));
#14626=DIRECTION('center_axis',(0.,1.,0.));
#14627=DIRECTION('ref_axis',(1.22464679914735E-16,0.,-1.));
#14628=DIRECTION('',(0.,1.,0.));
#14629=DIRECTION('',(0.,1.,0.));
#14630=DIRECTION('center_axis',(0.992484598701499,0.,0.122369609545525));
#14631=DIRECTION('ref_axis',(0.122369609545525,0.,-0.992484598701499));
#14632=DIRECTION('center_axis',(0.992484598701499,0.,-0.122369609545525));
#14633=DIRECTION('ref_axis',(-0.122369609545525,0.,-0.992484598701499));
#14634=DIRECTION('axis',(0.,0.,1.));
#14635=DIRECTION('refdir',(1.,0.,0.));
#14636=DIRECTION('axis',(0.,0.,1.));
#14637=DIRECTION('refdir',(1.,0.,0.));
#14638=DIRECTION('center_axis',(1.,0.,0.));
#14639=DIRECTION('ref_axis',(0.,0.,-1.));
#14640=DIRECTION('center_axis',(-1.,0.,0.));
#14641=DIRECTION('ref_axis',(0.,0.,-1.));
#14642=DIRECTION('',(1.,0.,0.));
#14643=DIRECTION('center_axis',(1.,0.,0.));
#14644=DIRECTION('ref_axis',(0.,0.,1.));
#14645=DIRECTION('center_axis',(1.,0.,0.));
#14646=DIRECTION('ref_axis',(0.,0.,-1.));
#14647=DIRECTION('center_axis',(-1.,0.,0.));
#14648=DIRECTION('ref_axis',(0.,0.,-1.));
#14649=DIRECTION('',(1.,0.,0.));
#14650=DIRECTION('center_axis',(1.,0.,0.));
#14651=DIRECTION('ref_axis',(0.,0.,-1.));
#14652=DIRECTION('center_axis',(1.,0.,0.));
#14653=DIRECTION('ref_axis',(0.,0.,-1.));
#14654=DIRECTION('center_axis',(-1.,0.,0.));
#14655=DIRECTION('ref_axis',(0.,0.,-1.));
#14656=DIRECTION('',(1.,0.,0.));
#14657=DIRECTION('center_axis',(1.,0.,0.));
#14658=DIRECTION('ref_axis',(0.,0.,-1.));
#14659=DIRECTION('center_axis',(0.,1.,0.));
#14660=DIRECTION('ref_axis',(0.,0.,1.));
#14661=DIRECTION('center_axis',(3.46944695195361E-16,1.,0.));
#14662=DIRECTION('ref_axis',(-1.,3.46944695195361E-16,0.));
#14663=DIRECTION('',(-1.73472347597681E-16,1.,0.));
#14664=DIRECTION('center_axis',(1.73472347597681E-16,-1.,0.));
#14665=DIRECTION('ref_axis',(1.,1.73472347597681E-16,0.));
#14666=DIRECTION('',(0.,-1.,0.));
#14667=DIRECTION('center_axis',(0.,1.,0.));
#14668=DIRECTION('ref_axis',(0.,0.,1.));
#14669=DIRECTION('center_axis',(3.46944695195361E-16,1.,0.));
#14670=DIRECTION('ref_axis',(-1.,3.46944695195361E-16,0.));
#14671=DIRECTION('',(0.,1.,0.));
#14672=DIRECTION('center_axis',(1.73472347597681E-16,-1.,0.));
#14673=DIRECTION('ref_axis',(1.,1.73472347597681E-16,0.));
#14674=DIRECTION('center_axis',(0.,-1.,0.));
#14675=DIRECTION('ref_axis',(0.,0.,-1.));
#14676=DIRECTION('center_axis',(0.,1.,0.));
#14677=DIRECTION('ref_axis',(0.,0.,-1.));
#14678=DIRECTION('',(0.,-1.,0.));
#14679=DIRECTION('center_axis',(0.,-1.,0.));
#14680=DIRECTION('ref_axis',(0.,0.,1.));
#14681=DIRECTION('center_axis',(-1.,0.,0.));
#14682=DIRECTION('ref_axis',(0.,0.,1.));
#14683=DIRECTION('',(0.,0.,-1.));
#14684=DIRECTION('',(0.,-1.,5.01544256350842E-32));
#14685=DIRECTION('',(0.,0.,-1.));
#14686=DIRECTION('',(0.,0.707106781186548,0.707106781186548));
#14687=DIRECTION('',(0.,0.,-1.));
#14688=DIRECTION('',(0.,0.707106781186546,-0.707106781186549));
#14689=DIRECTION('',(0.,-1.,0.));
#14690=DIRECTION('',(0.,0.707106781186547,0.707106781186547));
#14691=DIRECTION('',(0.,0.,-1.));
#14692=DIRECTION('',(0.,0.707106781186547,-0.707106781186548));
#14693=DIRECTION('center_axis',(0.,1.,0.));
#14694=DIRECTION('ref_axis',(0.,0.,1.));
#14695=DIRECTION('',(-1.,0.,0.));
#14696=DIRECTION('',(-1.,0.,0.));
#14697=DIRECTION('',(0.,0.,1.));
#14698=DIRECTION('center_axis',(0.,1.,0.));
#14699=DIRECTION('ref_axis',(0.,0.,1.));
#14700=DIRECTION('',(-1.,0.,0.));
#14701=DIRECTION('',(0.,0.,1.));
#14702=DIRECTION('',(1.,0.,0.));
#14703=DIRECTION('center_axis',(-4.00320802148494E-16,0.,-1.));
#14704=DIRECTION('ref_axis',(-1.,0.,4.00320802148494E-16));
#14705=DIRECTION('',(-1.,0.,4.00320802148494E-16));
#14706=DIRECTION('',(0.,1.,0.));
#14707=DIRECTION('',(1.,0.,-4.00320802148494E-16));
#14708=DIRECTION('',(0.,-1.,0.));
#14709=DIRECTION('center_axis',(0.,0.,1.));
#14710=DIRECTION('ref_axis',(1.,0.,0.));
#14711=DIRECTION('',(-1.,0.,0.));
#14712=DIRECTION('',(0.,-1.,0.));
#14713=DIRECTION('',(1.,0.,0.));
#14714=DIRECTION('center_axis',(1.,0.,0.));
#14715=DIRECTION('ref_axis',(0.,0.,-1.));
#14716=DIRECTION('',(0.,-0.707106781186548,-0.707106781186548));
#14717=DIRECTION('',(0.,0.,-1.));
#14718=DIRECTION('',(0.,1.,0.));
#14719=DIRECTION('',(0.,0.,-1.));
#14720=DIRECTION('',(0.,-0.707106781186547,0.707106781186548));
#14721=DIRECTION('',(0.,-0.707106781186547,-0.707106781186547));
#14722=DIRECTION('',(0.,-0.707106781186546,0.707106781186549));
#14723=DIRECTION('center_axis',(0.,0.,1.));
#14724=DIRECTION('ref_axis',(1.,0.,0.));
#14725=DIRECTION('',(-1.,0.,0.));
#14726=DIRECTION('',(0.,-1.,0.));
#14727=DIRECTION('',(1.,0.,0.));
#14728=DIRECTION('',(0.,-1.,0.));
#14729=DIRECTION('center_axis',(0.,-1.,0.));
#14730=DIRECTION('ref_axis',(0.,0.,-1.));
#14731=DIRECTION('center_axis',(0.,-1.,0.));
#14732=DIRECTION('ref_axis',(0.,0.,1.));
#14733=DIRECTION('center_axis',(0.,1.,0.));
#14734=DIRECTION('ref_axis',(0.,0.,-1.));
#14735=DIRECTION('center_axis',(0.,0.707106781186549,0.707106781186546));
#14736=DIRECTION('ref_axis',(-1.,0.,0.));
#14737=DIRECTION('center_axis',(0.,0.707106781186548,-0.707106781186548));
#14738=DIRECTION('ref_axis',(1.,0.,0.));
#14739=DIRECTION('center_axis',(0.,-1.,0.));
#14740=DIRECTION('ref_axis',(0.,0.,-1.));
#14741=DIRECTION('center_axis',(1.73472347597681E-16,-1.,0.));
#14742=DIRECTION('ref_axis',(1.,1.73472347597681E-16,0.));
#14743=DIRECTION('',(1.,2.89120579329468E-16,-2.89120579329468E-16));
#14744=DIRECTION('center_axis',(1.73472347597681E-16,-1.,0.));
#14745=DIRECTION('ref_axis',(1.,1.73472347597681E-16,0.));
#14746=DIRECTION('',(-1.,-1.73472347597681E-16,1.73472347597681E-16));
#14747=DIRECTION('center_axis',(0.,-1.,0.));
#14748=DIRECTION('ref_axis',(0.,0.,-1.));
#14749=DIRECTION('center_axis',(3.46944695195361E-16,1.,0.));
#14750=DIRECTION('ref_axis',(-1.,3.46944695195361E-16,0.));
#14751=DIRECTION('',(-1.,3.46944695195361E-16,2.89120579329468E-16));
#14752=DIRECTION('center_axis',(0.,1.,0.));
#14753=DIRECTION('ref_axis',(0.,0.,1.));
#14754=DIRECTION('center_axis',(0.,1.,0.));
#14755=DIRECTION('ref_axis',(0.,0.,1.));
#14756=DIRECTION('',(-1.,3.46944695195361E-16,3.46944695195361E-16));
#14757=DIRECTION('center_axis',(3.46944695195361E-16,1.,0.));
#14758=DIRECTION('ref_axis',(-1.,3.46944695195361E-16,0.));
#14759=DIRECTION('center_axis',(0.,1.,0.));
#14760=DIRECTION('ref_axis',(0.,0.,1.));
#14761=DIRECTION('center_axis',(0.,-0.707106781186548,-0.707106781186547));
#14762=DIRECTION('ref_axis',(0.,0.707106781186547,-0.707106781186548));
#14763=DIRECTION('center_axis',(0.,0.707106781186547,-0.707106781186548));
#14764=DIRECTION('ref_axis',(0.,0.707106781186548,0.707106781186547));
#14765=DIRECTION('center_axis',(2.89120579329468E-16,5.01544256350842E-32,
1.));
#14766=DIRECTION('ref_axis',(1.,-1.72766579818696E-64,-2.89120579329468E-16));
#14767=DIRECTION('',(0.,1.,-5.01544256350842E-32));
#14768=DIRECTION('center_axis',(0.,-1.,5.01544256350842E-32));
#14769=DIRECTION('ref_axis',(0.,-5.01544256350842E-32,-1.));
#14770=DIRECTION('center_axis',(0.,1.,0.));
#14771=DIRECTION('ref_axis',(0.,0.,1.));
#14772=DIRECTION('axis',(0.,0.,1.));
#14773=DIRECTION('refdir',(1.,0.,0.));
#14774=DIRECTION('center_axis',(-1.,0.,0.));
#14775=DIRECTION('ref_axis',(0.,0.,1.));
#14776=DIRECTION('',(0.,1.,0.));
#14777=DIRECTION('',(0.,0.,-1.));
#14778=DIRECTION('',(0.,1.,0.));
#14779=DIRECTION('',(0.,0.,-1.));
#14780=DIRECTION('center_axis',(0.,-1.,0.));
#14781=DIRECTION('ref_axis',(0.,0.,-1.));
#14782=DIRECTION('',(-1.,0.,0.));
#14783=DIRECTION('',(0.,0.,-1.));
#14784=DIRECTION('',(-1.,0.,0.));
#14785=DIRECTION('center_axis',(1.,3.46944695195361E-16,0.));
#14786=DIRECTION('ref_axis',(-3.46944695195361E-16,1.,0.));
#14787=DIRECTION('',(3.46944695195361E-16,-1.,0.));
#14788=DIRECTION('',(0.,0.,-1.));
#14789=DIRECTION('',(3.46944695195361E-16,-1.,0.));
#14790=DIRECTION('center_axis',(0.,1.,0.));
#14791=DIRECTION('ref_axis',(0.,0.,1.));
#14792=DIRECTION('',(1.,0.,0.));
#14793=DIRECTION('',(1.,0.,0.));
#14794=DIRECTION('center_axis',(0.,0.,1.));
#14795=DIRECTION('ref_axis',(1.,0.,0.));
#14796=DIRECTION('center_axis',(0.,0.,1.));
#14797=DIRECTION('ref_axis',(1.,0.,0.));
#14798=DIRECTION('axis',(0.,0.,1.));
#14799=DIRECTION('refdir',(1.,0.,0.));
#14800=DIRECTION('axis',(0.,0.,1.));
#14801=DIRECTION('refdir',(1.,0.,0.));
#14802=DIRECTION('center_axis',(0.,1.,0.));
#14803=DIRECTION('ref_axis',(0.,0.,1.));
#14804=DIRECTION('center_axis',(6.93889390390722E-17,-1.,0.));
#14805=DIRECTION('ref_axis',(-1.,-6.93889390390722E-17,0.));
#14806=DIRECTION('',(0.,1.,0.));
#14807=DIRECTION('center_axis',(6.93889390390722E-17,1.,0.));
#14808=DIRECTION('ref_axis',(1.,-6.93889390390722E-17,0.));
#14809=DIRECTION('center_axis',(0.,1.,0.));
#14810=DIRECTION('ref_axis',(0.,0.,1.));
#14811=DIRECTION('center_axis',(0.,1.,0.));
#14812=DIRECTION('ref_axis',(0.,0.,1.));
#14813=DIRECTION('',(0.,1.,0.));
#14814=DIRECTION('center_axis',(0.,-1.,0.));
#14815=DIRECTION('ref_axis',(0.,0.,-1.));
#14816=DIRECTION('center_axis',(0.,1.,0.));
#14817=DIRECTION('ref_axis',(0.,0.,1.));
#14818=DIRECTION('center_axis',(0.,1.,0.));
#14819=DIRECTION('ref_axis',(0.,0.,1.));
#14820=DIRECTION('',(0.,1.,0.));
#14821=DIRECTION('center_axis',(0.,1.,0.));
#14822=DIRECTION('ref_axis',(0.,0.,1.));
#14823=DIRECTION('center_axis',(0.,1.,0.));
#14824=DIRECTION('ref_axis',(0.,0.,1.));
#14825=DIRECTION('center_axis',(0.,1.,0.));
#14826=DIRECTION('ref_axis',(0.,0.,1.));
#14827=DIRECTION('',(0.,1.,0.));
#14828=DIRECTION('center_axis',(0.,-1.,0.));
#14829=DIRECTION('ref_axis',(0.,0.,-1.));
#14830=DIRECTION('center_axis',(0.,1.,0.));
#14831=DIRECTION('ref_axis',(0.,0.,1.));
#14832=DIRECTION('center_axis',(0.,1.,0.));
#14833=DIRECTION('ref_axis',(0.,0.,1.));
#14834=DIRECTION('',(0.,1.,0.));
#14835=DIRECTION('center_axis',(0.,1.,0.));
#14836=DIRECTION('ref_axis',(0.,0.,1.));
#14837=DIRECTION('center_axis',(1.,0.,0.));
#14838=DIRECTION('ref_axis',(0.,0.,-1.));
#14839=DIRECTION('',(0.,0.,-1.));
#14840=DIRECTION('',(0.,1.,0.));
#14841=DIRECTION('',(0.,0.,-1.));
#14842=DIRECTION('',(0.,-1.,0.));
#14843=DIRECTION('center_axis',(0.,1.,0.));
#14844=DIRECTION('ref_axis',(0.,0.,1.));
#14845=DIRECTION('',(1.,0.,0.));
#14846=DIRECTION('',(-0.707106781186546,0.,-0.707106781186549));
#14847=DIRECTION('',(0.707106781186548,0.,-0.707106781186547));
#14848=DIRECTION('',(1.,0.,0.));
#14849=DIRECTION('',(0.,0.,-1.));
#14850=DIRECTION('center_axis',(1.,3.06127672231201E-16,0.));
#14851=DIRECTION('ref_axis',(-3.06127672231201E-16,1.,0.));
#14852=DIRECTION('',(3.06127672231201E-16,-1.,0.));
#14853=DIRECTION('',(0.,0.,-1.));
#14854=DIRECTION('',(3.06127672231201E-16,-1.,0.));
#14855=DIRECTION('center_axis',(0.,-1.,0.));
#14856=DIRECTION('ref_axis',(0.,0.,-1.));
#14857=DIRECTION('',(0.,0.,-1.));
#14858=DIRECTION('',(0.707106781186546,0.,0.707106781186549));
#14859=DIRECTION('',(-1.,0.,0.));
#14860=DIRECTION('',(-1.,0.,0.));
#14861=DIRECTION('',(-0.707106781186548,0.,0.707106781186547));
#14862=DIRECTION('center_axis',(1.,0.,0.));
#14863=DIRECTION('ref_axis',(0.,0.,-1.));
#14864=DIRECTION('',(0.,0.,-1.));
#14865=DIRECTION('',(0.,1.,0.));
#14866=DIRECTION('',(0.,-1.,0.));
#14867=DIRECTION('center_axis',(0.,1.,0.));
#14868=DIRECTION('ref_axis',(0.,0.,1.));
#14869=DIRECTION('',(1.,0.,0.));
#14870=DIRECTION('',(0.,0.,1.));
#14871=DIRECTION('',(1.,0.,0.));
#14872=DIRECTION('',(-0.707106781186546,0.,-0.707106781186549));
#14873=DIRECTION('',(0.707106781186548,0.,-0.707106781186547));
#14874=DIRECTION('center_axis',(0.,-1.,0.));
#14875=DIRECTION('ref_axis',(0.,0.,-1.));
#14876=DIRECTION('',(-1.,0.,0.));
#14877=DIRECTION('',(0.,0.,-1.));
#14878=DIRECTION('',(-1.,0.,0.));
#14879=DIRECTION('',(-0.707106781186548,0.,0.707106781186547));
#14880=DIRECTION('',(0.707106781186546,0.,0.707106781186549));
#14881=DIRECTION('center_axis',(0.,0.,1.));
#14882=DIRECTION('ref_axis',(1.,0.,0.));
#14883=DIRECTION('',(0.707106781186545,0.70710678118655,0.));
#14884=DIRECTION('',(0.,1.,0.));
#14885=DIRECTION('',(0.,1.,0.));
#14886=DIRECTION('',(-5.71424710475988E-16,-1.,0.));
#14887=DIRECTION('',(-0.707106781186549,0.707106781186546,0.));
#14888=DIRECTION('',(0.,-1.,0.));
#14889=DIRECTION('',(0.,-1.,0.));
#14890=DIRECTION('center_axis',(0.,0.,1.));
#14891=DIRECTION('ref_axis',(1.,0.,0.));
#14892=DIRECTION('',(0.,1.,0.));
#14893=DIRECTION('',(-0.707106781186545,-0.70710678118655,0.));
#14894=DIRECTION('',(0.,1.,0.));
#14895=DIRECTION('',(0.,1.,0.));
#14896=DIRECTION('',(0.707106781186549,-0.707106781186546,0.));
#14897=DIRECTION('',(-5.71424710475988E-16,-1.,0.));
#14898=DIRECTION('',(0.,1.,0.));
#14899=DIRECTION('center_axis',(-0.707106781186549,0.,0.707106781186546));
#14900=DIRECTION('ref_axis',(0.,1.,0.));
#14901=DIRECTION('center_axis',(0.707106781186547,0.,0.707106781186548));
#14902=DIRECTION('ref_axis',(0.,-1.,0.));
#14903=DIRECTION('center_axis',(-0.707106781186549,0.,0.707106781186546));
#14904=DIRECTION('ref_axis',(0.,1.,0.));
#14905=DIRECTION('center_axis',(0.707106781186547,0.,0.707106781186548));
#14906=DIRECTION('ref_axis',(0.,-1.,0.));
#14907=DIRECTION('center_axis',(0.,1.,0.));
#14908=DIRECTION('ref_axis',(0.,0.,1.));
#14909=DIRECTION('center_axis',(6.93889390390722E-17,-1.,0.));
#14910=DIRECTION('ref_axis',(-1.,-6.93889390390722E-17,0.));
#14911=DIRECTION('',(0.,1.,0.));
#14912=DIRECTION('center_axis',(6.93889390390722E-17,1.,0.));
#14913=DIRECTION('ref_axis',(1.,-6.93889390390723E-17,0.));
#14914=DIRECTION('',(0.,1.,0.));
#14915=DIRECTION('center_axis',(0.,0.,1.));
#14916=DIRECTION('ref_axis',(1.,0.,0.));
#14917=DIRECTION('',(-1.,-6.93889390390722E-17,0.));
#14918=DIRECTION('',(1.,-6.93889390390722E-17,0.));
#14919=DIRECTION('',(0.,-1.,0.));
#14920=DIRECTION('center_axis',(0.,0.,-1.));
#14921=DIRECTION('ref_axis',(-1.,0.,0.));
#14922=DIRECTION('',(1.,6.93889390390722E-17,0.));
#14923=DIRECTION('',(0.,1.,0.));
#14924=DIRECTION('',(-1.,6.93889390390722E-17,0.));
#14925=DIRECTION('center_axis',(0.,1.,0.));
#14926=DIRECTION('ref_axis',(0.,0.,1.));
#14927=DIRECTION('center_axis',(6.93889390390722E-17,-1.,0.));
#14928=DIRECTION('ref_axis',(-1.,-6.93889390390722E-17,8.67361737988404E-16));
#14929=DIRECTION('center_axis',(6.93889390390722E-17,1.,0.));
#14930=DIRECTION('ref_axis',(1.,-6.93889390390722E-17,0.));
#14931=DIRECTION('center_axis',(0.,1.,0.));
#14932=DIRECTION('ref_axis',(0.,0.,1.));
#14933=DIRECTION('center_axis',(6.93889390390722E-17,-1.,0.));
#14934=DIRECTION('ref_axis',(-1.,-6.93889390390722E-17,6.93889390390723E-16));
#14935=DIRECTION('center_axis',(6.93889390390722E-17,1.,0.));
#14936=DIRECTION('ref_axis',(1.,-6.93889390390722E-17,0.));
#14937=DIRECTION('center_axis',(-6.93889390390722E-17,-1.,0.));
#14938=DIRECTION('ref_axis',(1.,-6.93889390390723E-17,0.));
#14939=DIRECTION('',(0.,0.,1.));
#14940=DIRECTION('center_axis',(-1.,5.71424710475987E-16,0.));
#14941=DIRECTION('ref_axis',(-5.71424710475987E-16,-1.,0.));
#14942=DIRECTION('',(0.,0.,1.));
#14943=DIRECTION('center_axis',(-6.93889390390722E-17,1.,0.));
#14944=DIRECTION('ref_axis',(-1.,-6.93889390390723E-17,0.));
#14945=DIRECTION('',(0.,0.,1.));
#14946=DIRECTION('center_axis',(-1.,-5.71424710475987E-16,0.));
#14947=DIRECTION('ref_axis',(5.71424710475987E-16,-1.,0.));
#14948=DIRECTION('',(0.,0.,-1.));
#14949=DIRECTION('center_axis',(-0.70710678118655,0.707106781186545,0.));
#14950=DIRECTION('ref_axis',(0.,0.,1.));
#14951=DIRECTION('center_axis',(-0.707106781186546,-0.707106781186549,0.));
#14952=DIRECTION('ref_axis',(0.,0.,1.));
#14953=DIRECTION('axis',(0.,0.,1.));
#14954=DIRECTION('refdir',(1.,0.,0.));
#14955=DIRECTION('center_axis',(0.,0.,1.));
#14956=DIRECTION('ref_axis',(1.,0.,0.));
#14957=DIRECTION('center_axis',(0.,0.,1.));
#14958=DIRECTION('ref_axis',(1.,0.,0.));
#14959=DIRECTION('center_axis',(-1.22464679914735E-16,1.,0.));
#14960=DIRECTION('ref_axis',(-1.,-1.22464679914735E-16,0.));
#14961=DIRECTION('center_axis',(0.,0.,1.));
#14962=DIRECTION('ref_axis',(1.,0.,0.));
#14963=DIRECTION('center_axis',(0.,0.,1.));
#14964=DIRECTION('ref_axis',(1.,0.,0.));
#14965=DIRECTION('center_axis',(0.,0.,1.));
#14966=DIRECTION('ref_axis',(1.,0.,0.));
#14967=DIRECTION('',(-0.707106781186551,-8.65956056235498E-17,0.707106781186544));
#14968=DIRECTION('center_axis',(0.,0.,1.));
#14969=DIRECTION('ref_axis',(1.,0.,0.));
#14970=DIRECTION('center_axis',(0.,0.,1.));
#14971=DIRECTION('ref_axis',(1.,0.,0.));
#14972=DIRECTION('center_axis',(0.,0.,1.));
#14973=DIRECTION('ref_axis',(1.,0.,0.));
#14974=DIRECTION('center_axis',(0.,0.,1.));
#14975=DIRECTION('ref_axis',(1.,0.,0.));
#14976=DIRECTION('',(0.,0.,1.));
#14977=DIRECTION('center_axis',(0.,0.,-1.));
#14978=DIRECTION('ref_axis',(-1.,0.,0.));
#14979=DIRECTION('',(0.707106781186544,-8.65956056235489E-17,-0.707106781186551));
#14980=DIRECTION('center_axis',(0.,0.,1.));
#14981=DIRECTION('ref_axis',(1.,0.,0.));
#14982=DIRECTION('center_axis',(0.,0.,1.));
#14983=DIRECTION('ref_axis',(1.,0.,0.));
#14984=DIRECTION('',(0.,0.,-1.));
#14985=DIRECTION('center_axis',(0.,0.,1.));
#14986=DIRECTION('ref_axis',(1.,0.,0.));
#14987=DIRECTION('center_axis',(0.,0.,1.));
#14988=DIRECTION('ref_axis',(1.,0.,0.));
#14989=DIRECTION('center_axis',(0.,0.,1.));
#14990=DIRECTION('ref_axis',(1.,0.,0.));
#14991=DIRECTION('',(0.,0.,-1.));
#14992=DIRECTION('center_axis',(0.,0.,-1.));
#14993=DIRECTION('ref_axis',(-1.,0.,0.));
#14994=DIRECTION('center_axis',(0.,0.,1.));
#14995=DIRECTION('ref_axis',(1.,0.,0.));
#14996=DIRECTION('center_axis',(-1.,0.,0.));
#14997=DIRECTION('ref_axis',(0.,1.,0.));
#14998=DIRECTION('center_axis',(0.,1.22464679914735E-16,1.));
#14999=DIRECTION('ref_axis',(0.,-1.,1.22464679914735E-16));
#15000=DIRECTION('center_axis',(-0.866025403784438,0.500000000000001,0.));
#15001=DIRECTION('ref_axis',(0.500000000000001,0.866025403784438,0.));
#15002=DIRECTION('center_axis',(6.12323399573678E-17,1.06057523872491E-16,
1.));
#15003=DIRECTION('ref_axis',(-0.500000000000001,-0.866025403784438,1.22464679914735E-16));
#15004=DIRECTION('center_axis',(-0.499999999999998,0.86602540378444,0.));
#15005=DIRECTION('ref_axis',(0.86602540378444,0.499999999999998,0.));
#15006=DIRECTION('center_axis',(1.06057523872491E-16,6.12323399573674E-17,
1.));
#15007=DIRECTION('ref_axis',(-0.86602540378444,-0.499999999999998,1.22464679914735E-16));
#15008=DIRECTION('center_axis',(3.66483584538337E-15,1.,0.));
#15009=DIRECTION('ref_axis',(1.,-3.49148336110938E-15,0.));
#15010=DIRECTION('center_axis',(1.22464679914735E-16,-4.27583392245885E-31,
1.));
#15011=DIRECTION('ref_axis',(-1.,3.49148336110938E-15,1.22464679914735E-16));
#15012=DIRECTION('center_axis',(0.500000000000004,0.866025403784436,0.));
#15013=DIRECTION('ref_axis',(0.866025403784436,-0.500000000000004,0.));
#15014=DIRECTION('center_axis',(1.0605752387249E-16,-6.12323399573681E-17,
1.));
#15015=DIRECTION('ref_axis',(-0.866025403784436,0.500000000000004,1.22464679914735E-16));
#15016=DIRECTION('center_axis',(0.866025403784441,0.499999999999995,0.));
#15017=DIRECTION('ref_axis',(0.499999999999995,-0.866025403784441,0.));
#15018=DIRECTION('center_axis',(6.1232339957367E-17,-1.06057523872491E-16,
1.));
#15019=DIRECTION('ref_axis',(-0.499999999999995,0.866025403784441,1.22464679914735E-16));
#15020=DIRECTION('center_axis',(1.,-7.32967169076675E-15,0.));
#15021=DIRECTION('ref_axis',(-6.98296672221876E-15,-1.,0.));
#15022=DIRECTION('center_axis',(-8.55166784491769E-31,-1.22464679914735E-16,
1.));
#15023=DIRECTION('ref_axis',(6.98296672221877E-15,1.,1.22464679914735E-16));
#15024=DIRECTION('center_axis',(0.866025403784434,-0.500000000000008,0.));
#15025=DIRECTION('ref_axis',(-0.500000000000008,-0.866025403784434,0.));
#15026=DIRECTION('center_axis',(-6.12323399573685E-17,-1.0605752387249E-16,
1.));
#15027=DIRECTION('ref_axis',(0.500000000000007,0.866025403784434,1.22464679914735E-16));
#15028=DIRECTION('center_axis',(0.499999999999992,-0.866025403784443,0.));
#15029=DIRECTION('ref_axis',(-0.866025403784443,-0.499999999999992,0.));
#15030=DIRECTION('center_axis',(-1.06057523872491E-16,-6.12323399573666E-17,
1.));
#15031=DIRECTION('ref_axis',(0.866025403784443,0.499999999999992,1.22464679914735E-16));
#15032=DIRECTION('center_axis',(-1.02615403670734E-14,-1.,0.));
#15033=DIRECTION('ref_axis',(-1.,1.04744500833281E-14,0.));
#15034=DIRECTION('center_axis',(-1.22464679914735E-16,1.28275017673765E-30,
1.));
#15035=DIRECTION('ref_axis',(1.,-1.04744500833281E-14,1.22464679914735E-16));
#15036=DIRECTION('center_axis',(-0.50000000000001,-0.866025403784433,0.));
#15037=DIRECTION('ref_axis',(-0.866025403784433,0.50000000000001,0.));
#15038=DIRECTION('center_axis',(-1.0605752387249E-16,6.12323399573689E-17,
1.));
#15039=DIRECTION('ref_axis',(0.866025403784433,-0.50000000000001,1.22464679914735E-16));
#15040=DIRECTION('center_axis',(-0.866025403784445,-0.499999999999989,0.));
#15041=DIRECTION('ref_axis',(-0.499999999999989,0.866025403784445,0.));
#15042=DIRECTION('center_axis',(-6.12323399573663E-17,1.06057523872491E-16,
1.));
#15043=DIRECTION('ref_axis',(0.499999999999989,-0.866025403784445,1.22464679914735E-16));
#15044=DIRECTION('center_axis',(0.,0.,1.));
#15045=DIRECTION('ref_axis',(1.,0.,0.));
#15046=DIRECTION('center_axis',(0.,0.,1.));
#15047=DIRECTION('ref_axis',(1.,0.,0.));
#15048=DIRECTION('',(0.,0.,-1.));
#15049=DIRECTION('center_axis',(0.,0.,1.));
#15050=DIRECTION('ref_axis',(1.,0.,0.));
#15051=DIRECTION('center_axis',(0.,0.,1.));
#15052=DIRECTION('ref_axis',(1.,0.,0.));
#15053=DIRECTION('center_axis',(0.,0.,1.));
#15054=DIRECTION('ref_axis',(1.,0.,0.));
#15055=DIRECTION('',(0.,0.,1.));
#15056=DIRECTION('center_axis',(0.,0.,1.));
#15057=DIRECTION('ref_axis',(1.,0.,0.));
#15058=DIRECTION('center_axis',(0.,0.,-1.));
#15059=DIRECTION('ref_axis',(-1.,0.,0.));
#15060=DIRECTION('center_axis',(0.,0.,1.));
#15061=DIRECTION('ref_axis',(1.,0.,0.));
#15062=DIRECTION('center_axis',(0.,0.,1.));
#15063=DIRECTION('ref_axis',(1.,0.,0.));
#15064=DIRECTION('center_axis',(0.,0.,1.));
#15065=DIRECTION('ref_axis',(1.,0.,0.));
#15066=DIRECTION('',(0.,0.,-1.));
#15067=DIRECTION('center_axis',(0.,0.,1.));
#15068=DIRECTION('ref_axis',(1.,0.,0.));
#15069=DIRECTION('center_axis',(0.,0.,1.));
#15070=DIRECTION('ref_axis',(1.,0.,0.));
#15071=DIRECTION('center_axis',(0.,0.,1.));
#15072=DIRECTION('ref_axis',(1.,0.,0.));
#15073=DIRECTION('',(0.,0.,1.));
#15074=DIRECTION('center_axis',(0.,0.,1.));
#15075=DIRECTION('ref_axis',(1.,0.,0.));
#15076=DIRECTION('center_axis',(0.,0.,1.));
#15077=DIRECTION('ref_axis',(1.,0.,0.));
#15078=DIRECTION('center_axis',(0.,0.,-1.));
#15079=DIRECTION('ref_axis',(-1.,0.,0.));
#15080=DIRECTION('center_axis',(0.,0.,-1.));
#15081=DIRECTION('ref_axis',(-1.,0.,0.));
#15082=DIRECTION('center_axis',(0.,0.,-1.));
#15083=DIRECTION('ref_axis',(-1.,0.,0.));
#15084=DIRECTION('',(0.,0.,1.));
#15085=DIRECTION('center_axis',(0.,0.,-1.));
#15086=DIRECTION('ref_axis',(-1.,0.,0.));
#15087=DIRECTION('center_axis',(0.,0.,1.));
#15088=DIRECTION('ref_axis',(1.,0.,0.));
#15089=DIRECTION('center_axis',(0.,0.,1.));
#15090=DIRECTION('ref_axis',(1.,0.,0.));
#15091=DIRECTION('',(0.,0.,1.));
#15092=DIRECTION('center_axis',(0.,0.,1.));
#15093=DIRECTION('ref_axis',(1.,0.,0.));
#15094=DIRECTION('center_axis',(0.,0.,1.));
#15095=DIRECTION('ref_axis',(1.,0.,0.));
#15096=DIRECTION('center_axis',(0.,0.,1.));
#15097=DIRECTION('ref_axis',(1.,0.,0.));
#15098=DIRECTION('center_axis',(-1.22464679914735E-16,1.,0.));
#15099=DIRECTION('ref_axis',(-1.,-1.22464679914735E-16,0.));
#15100=DIRECTION('center_axis',(0.,0.,1.));
#15101=DIRECTION('ref_axis',(1.,0.,0.));
#15102=DIRECTION('center_axis',(0.,0.,1.));
#15103=DIRECTION('ref_axis',(1.,0.,0.));
#15104=DIRECTION('',(0.,0.,1.));
#15105=DIRECTION('center_axis',(0.,0.,1.));
#15106=DIRECTION('ref_axis',(1.,0.,0.));
#15107=DIRECTION('center_axis',(0.,0.,1.));
#15108=DIRECTION('ref_axis',(1.,0.,0.));
#15109=DIRECTION('center_axis',(0.,0.,1.));
#15110=DIRECTION('ref_axis',(1.,0.,0.));
#15111=DIRECTION('',(0.,0.,-1.));
#15112=DIRECTION('center_axis',(0.,0.,1.));
#15113=DIRECTION('ref_axis',(1.,0.,0.));
#15114=DIRECTION('center_axis',(0.,0.,-1.));
#15115=DIRECTION('ref_axis',(-1.,0.,0.));
#15116=DIRECTION('',(-0.707106781186546,8.65956056235491E-17,0.707106781186549));
#15117=DIRECTION('center_axis',(0.,0.,1.));
#15118=DIRECTION('ref_axis',(1.,0.,0.));
#15119=DIRECTION('center_axis',(0.,0.,1.));
#15120=DIRECTION('ref_axis',(1.,0.,0.));
#15121=DIRECTION('center_axis',(0.,0.,-1.));
#15122=DIRECTION('ref_axis',(-1.,0.,0.));
#15123=DIRECTION('center_axis',(0.,0.,1.));
#15124=DIRECTION('ref_axis',(1.,0.,0.));
#15125=DIRECTION('axis',(0.,0.,1.));
#15126=DIRECTION('refdir',(1.,0.,0.));
#15127=DIRECTION('center_axis',(0.,0.,-1.));
#15128=DIRECTION('ref_axis',(-1.,0.,0.));
#15129=DIRECTION('center_axis',(0.,0.,-1.));
#15130=DIRECTION('ref_axis',(-1.,0.,0.));
#15131=DIRECTION('',(0.,0.,1.));
#15132=DIRECTION('center_axis',(0.,0.,-1.));
#15133=DIRECTION('ref_axis',(-1.,0.,0.));
#15134=DIRECTION('center_axis',(0.,0.,-1.));
#15135=DIRECTION('ref_axis',(-1.,0.,0.));
#15136=DIRECTION('center_axis',(0.,0.,1.));
#15137=DIRECTION('ref_axis',(1.,0.,0.));
#15138=DIRECTION('',(0.,0.,-1.));
#15139=DIRECTION('center_axis',(0.,0.,1.));
#15140=DIRECTION('ref_axis',(1.,0.,0.));
#15141=DIRECTION('center_axis',(0.,0.,-1.));
#15142=DIRECTION('ref_axis',(-1.,0.,0.));
#15143=DIRECTION('center_axis',(0.,0.,-1.));
#15144=DIRECTION('ref_axis',(-1.,0.,0.));
#15145=DIRECTION('',(0.,0.,1.));
#15146=DIRECTION('center_axis',(0.,0.,1.));
#15147=DIRECTION('ref_axis',(1.,0.,0.));
#15148=DIRECTION('center_axis',(0.,0.,1.));
#15149=DIRECTION('ref_axis',(1.,0.,0.));
#15150=DIRECTION('center_axis',(0.,0.,1.));
#15151=DIRECTION('ref_axis',(1.,0.,0.));
#15152=DIRECTION('center_axis',(0.,0.,-1.));
#15153=DIRECTION('ref_axis',(-1.,0.,0.));
#15154=DIRECTION('axis',(0.,0.,1.));
#15155=DIRECTION('refdir',(1.,0.,0.));
#15156=DIRECTION('center_axis',(6.16297582203916E-33,-5.54667823983524E-32,
-1.));
#15157=DIRECTION('ref_axis',(-1.,-6.66133814775094E-16,-6.16297582203912E-33));
#15158=DIRECTION('center_axis',(6.16297582203915E-33,-6.77927340424307E-32,
-1.));
#15159=DIRECTION('ref_axis',(-1.,-6.66133814775094E-16,-6.16297582203911E-33));
#15160=DIRECTION('',(-6.16297582203916E-33,5.54667823983524E-32,1.));
#15161=DIRECTION('center_axis',(6.16297582203915E-33,-6.77927340424307E-32,
-1.));
#15162=DIRECTION('ref_axis',(-1.,-6.66133814775094E-16,-6.16297582203911E-33));
#15163=DIRECTION('center_axis',(6.16297582203915E-33,-6.77927340424307E-32,
-1.));
#15164=DIRECTION('ref_axis',(-1.,-6.66133814775094E-16,-6.16297582203911E-33));
#15165=DIRECTION('center_axis',(-6.16297582203915E-33,6.77927340424307E-32,
1.));
#15166=DIRECTION('ref_axis',(1.,6.66133814775094E-16,6.16297582203911E-33));
#15167=DIRECTION('',(6.16297582203915E-33,-6.77927340424307E-32,-1.));
#15168=DIRECTION('center_axis',(-6.16297582203915E-33,6.77927340424307E-32,
1.));
#15169=DIRECTION('ref_axis',(1.,6.66133814775094E-16,6.16297582203911E-33));
#15170=DIRECTION('center_axis',(6.16297582203915E-33,-6.77927340424307E-32,
-1.));
#15171=DIRECTION('ref_axis',(-1.,-6.66133814775094E-16,-6.16297582203911E-33));
#15172=DIRECTION('center_axis',(6.16297582203915E-33,-6.77927340424307E-32,
-1.));
#15173=DIRECTION('ref_axis',(-1.,-6.66133814775094E-16,-6.16297582203911E-33));
#15174=DIRECTION('',(-6.16297582203915E-33,6.77927340424307E-32,1.));
#15175=DIRECTION('center_axis',(-6.16297582203915E-33,6.77927340424307E-32,
1.));
#15176=DIRECTION('ref_axis',(1.,6.66133814775094E-16,6.16297582203911E-33));
#15177=DIRECTION('center_axis',(1.54074395550978E-32,6.77927340424307E-32,
1.));
#15178=DIRECTION('ref_axis',(1.,6.66133814775094E-16,-1.54074395550979E-32));
#15179=DIRECTION('center_axis',(1.54074395550978E-32,6.77927340424307E-32,
1.));
#15180=DIRECTION('ref_axis',(1.,6.66133814775094E-16,-1.54074395550979E-32));
#15181=DIRECTION('center_axis',(-1.54074395550978E-32,-6.77927340424307E-32,
-1.));
#15182=DIRECTION('ref_axis',(-1.,-6.66133814775094E-16,1.54074395550979E-32));
#15183=DIRECTION('',(-2.61615738687592E-68,-5.49392910365049E-26,1.));
#15184=DIRECTION('',(1.,7.8689738112411E-27,4.3231584237441E-52));
#15185=DIRECTION('',(-7.8689738112411E-27,-1.,5.49392910365049E-26));
#15186=DIRECTION('',(1.,-7.8689738112411E-27,8.6463168474882E-52));
#15187=DIRECTION('',(-1.,-1.61723261012338E-17,-2.35040441972026E-17));
#15188=DIRECTION('',(-2.35040441972026E-17,-1.11022302517455E-16,1.));
#15189=DIRECTION('',(-5.55111512391268E-17,-1.,4.16333634783827E-17));
#15190=DIRECTION('',(-0.109827878837254,4.74781794769823E-17,0.993950621022045));
#15191=DIRECTION('',(7.86897446673577E-27,1.,1.11022302407576E-16));
#15192=DIRECTION('',(0.939291267301778,3.80940663536785E-17,-0.343120846307275));
#15193=DIRECTION('',(7.8689738112411E-27,1.,-5.49392910365049E-26));
#15194=DIRECTION('',(0.579242738400294,-4.93420896541648E-26,-0.815155107946045));
#15195=DIRECTION('',(2.15506501834135E-18,1.,1.24911720199028E-16));
#15196=DIRECTION('',(0.99734967099538,6.93889389206186E-18,-0.072757362276314));
#15197=DIRECTION('',(-7.8689738112411E-27,-1.,5.49392910365049E-26));
#15198=DIRECTION('',(0.997707166488188,-4.13271034572545E-27,0.0676787258901295));
#15199=DIRECTION('',(-5.55111512391268E-17,-1.,4.16333634783827E-17));
#15200=DIRECTION('',(-0.109827878837254,4.74781794769823E-17,0.993950621022045));
#15201=DIRECTION('',(7.86897446673577E-27,1.,1.11022302407576E-16));
#15202=DIRECTION('',(0.939291267301778,3.80940663536785E-17,-0.343120846307275));
#15203=DIRECTION('',(-1.38777878078145E-17,-1.88605536453525E-17,1.));
#15204=DIRECTION('',(1.,5.46136239248286E-17,1.38777878078145E-17));
#15205=DIRECTION('',(-5.46136239248286E-17,-1.,1.88605536453525E-17));
#15206=DIRECTION('',(1.,-5.46136239248286E-17,-1.38777878078145E-17));
#15207=DIRECTION('',(5.46136239248286E-17,1.,-1.88605536453525E-17));
#15208=DIRECTION('',(1.,-5.46136239248286E-17,-1.38777878078145E-17));
#15209=DIRECTION('',(-5.46136239248286E-17,-1.,1.88605536453525E-17));
#15210=DIRECTION('',(1.,-5.46136239248286E-17,-1.38777878078145E-17));
#15211=DIRECTION('',(5.67358956919808E-17,1.,-5.42380508805648E-17));
#15212=DIRECTION('',(0.913936162522886,-7.38659319477158E-17,-0.405857968793199));
#15213=DIRECTION('axis',(0.,0.,1.));
#15214=DIRECTION('refdir',(1.,0.,0.));
#15215=DIRECTION('center_axis',(0.,1.,0.));
#15216=DIRECTION('ref_axis',(0.,0.,1.));
#15217=DIRECTION('center_axis',(0.,1.,0.));
#15218=DIRECTION('ref_axis',(0.,0.,1.));
#15219=DIRECTION('',(-8.65956056235496E-17,0.707106781186545,-0.70710678118655));
#15220=DIRECTION('center_axis',(0.,1.,0.));
#15221=DIRECTION('ref_axis',(0.,0.,1.));
#15222=DIRECTION('center_axis',(0.,1.,0.));
#15223=DIRECTION('ref_axis',(0.,0.,1.));
#15224=DIRECTION('center_axis',(0.,1.,0.));
#15225=DIRECTION('ref_axis',(0.,0.,1.));
#15226=DIRECTION('',(0.,1.,0.));
#15227=DIRECTION('center_axis',(0.,1.,0.));
#15228=DIRECTION('ref_axis',(0.,0.,1.));
#15229=DIRECTION('center_axis',(0.,1.,0.));
#15230=DIRECTION('ref_axis',(0.,0.,1.));
#15231=DIRECTION('',(-8.65956056235496E-17,0.707106781186545,-0.70710678118655));
#15232=DIRECTION('center_axis',(0.,1.,0.));
#15233=DIRECTION('ref_axis',(0.,0.,1.));
#15234=DIRECTION('center_axis',(0.,1.,0.));
#15235=DIRECTION('ref_axis',(0.,0.,1.));
#15236=DIRECTION('center_axis',(0.,1.,0.));
#15237=DIRECTION('ref_axis',(0.,0.,1.));
#15238=DIRECTION('',(0.,1.,0.));
#15239=DIRECTION('center_axis',(0.,-1.,0.));
#15240=DIRECTION('ref_axis',(0.,0.,-1.));
#15241=DIRECTION('center_axis',(0.,1.,0.));
#15242=DIRECTION('ref_axis',(0.,0.,1.));
#15243=DIRECTION('',(0.,-1.,0.));
#15244=DIRECTION('center_axis',(0.,1.,0.));
#15245=DIRECTION('ref_axis',(0.,0.,1.));
#15246=DIRECTION('',(0.,-1.,0.));
#15247=DIRECTION('center_axis',(0.,1.,0.));
#15248=DIRECTION('ref_axis',(0.,0.,1.));
#15249=DIRECTION('center_axis',(0.,1.,0.));
#15250=DIRECTION('ref_axis',(0.,0.,1.));
#15251=DIRECTION('',(0.,0.,-1.));
#15252=DIRECTION('',(0.,0.,1.));
#15253=DIRECTION('center_axis',(0.,1.,0.));
#15254=DIRECTION('ref_axis',(0.,0.,1.));
#15255=DIRECTION('center_axis',(0.,1.,0.));
#15256=DIRECTION('ref_axis',(0.,0.,1.));
#15257=DIRECTION('',(0.,0.,1.));
#15258=DIRECTION('',(0.,0.,-1.));
#15259=DIRECTION('center_axis',(0.,-1.,0.));
#15260=DIRECTION('ref_axis',(1.22464679914735E-16,0.,1.));
#15261=DIRECTION('',(0.,-1.,0.));
#15262=DIRECTION('',(0.,-1.,0.));
#15263=DIRECTION('center_axis',(-1.,0.,0.));
#15264=DIRECTION('ref_axis',(0.,0.,1.));
#15265=DIRECTION('center_axis',(1.,0.,0.));
#15266=DIRECTION('ref_axis',(0.,0.,-1.));
#15267=DIRECTION('axis',(0.,0.,1.));
#15268=DIRECTION('refdir',(1.,0.,0.));
#15269=DIRECTION('center_axis',(-1.,0.,0.));
#15270=DIRECTION('ref_axis',(0.,0.,1.));
#15271=DIRECTION('',(-0.500000000000004,-1.0605752387249E-16,-0.866025403784436));
#15272=DIRECTION('center_axis',(-1.,0.,0.));
#15273=DIRECTION('ref_axis',(0.,0.,1.));
#15274=DIRECTION('center_axis',(-1.,0.,0.));
#15275=DIRECTION('ref_axis',(0.,0.,1.));
#15276=DIRECTION('center_axis',(-1.,0.,0.));
#15277=DIRECTION('ref_axis',(0.,0.,1.));
#15278=DIRECTION('center_axis',(-1.,0.,0.));
#15279=DIRECTION('ref_axis',(0.,0.,1.));
#15280=DIRECTION('center_axis',(-1.,0.,0.));
#15281=DIRECTION('ref_axis',(0.,0.,1.));
#15282=DIRECTION('center_axis',(-1.,0.,0.));
#15283=DIRECTION('ref_axis',(0.,0.,1.));
#15284=DIRECTION('center_axis',(-1.,0.,0.));
#15285=DIRECTION('ref_axis',(0.,0.,1.));
#15286=DIRECTION('center_axis',(-1.,0.,0.));
#15287=DIRECTION('ref_axis',(0.,0.,1.));
#15288=DIRECTION('center_axis',(0.,1.,-1.22464679914735E-16));
#15289=DIRECTION('ref_axis',(0.,-1.22464679914735E-16,-1.));
#15290=DIRECTION('center_axis',(1.,0.,0.));
#15291=DIRECTION('ref_axis',(0.,0.,1.));
#15292=DIRECTION('center_axis',(-1.,0.,0.));
#15293=DIRECTION('ref_axis',(0.,0.,1.));
#15294=DIRECTION('center_axis',(-1.,0.,0.));
#15295=DIRECTION('ref_axis',(0.,0.,1.));
#15296=DIRECTION('',(1.,0.,0.));
#15297=DIRECTION('center_axis',(-1.,0.,0.));
#15298=DIRECTION('ref_axis',(0.,0.,1.));
#15299=DIRECTION('center_axis',(-1.,0.,0.));
#15300=DIRECTION('ref_axis',(0.,0.,1.));
#15301=DIRECTION('',(0.707106781186546,8.65956056235496E-17,0.70710678118655));
#15302=DIRECTION('center_axis',(-1.,0.,0.));
#15303=DIRECTION('ref_axis',(0.,0.,1.));
#15304=DIRECTION('',(1.,0.,0.));
#15305=DIRECTION('center_axis',(-1.,0.,0.));
#15306=DIRECTION('ref_axis',(0.,0.,1.));
#15307=DIRECTION('center_axis',(-1.,0.,0.));
#15308=DIRECTION('ref_axis',(0.,0.,1.));
#15309=DIRECTION('',(0.707106781186526,8.65956056235519E-17,0.707106781186569));
#15310=DIRECTION('center_axis',(-1.,0.,0.));
#15311=DIRECTION('ref_axis',(0.,0.,1.));
#15312=DIRECTION('center_axis',(-1.,0.,0.));
#15313=DIRECTION('ref_axis',(0.,0.,1.));
#15314=DIRECTION('',(0.,-0.500000000000001,-0.866025403784438));
#15315=DIRECTION('',(0.,0.5,-0.866025403784438));
#15316=DIRECTION('',(0.,1.,6.00925839494864E-16));
#15317=DIRECTION('',(0.,0.5,0.866025403784438));
#15318=DIRECTION('',(0.,-0.5,0.866025403784438));
#15319=DIRECTION('',(0.,-1.,0.));
#15320=DIRECTION('center_axis',(1.,0.,0.));
#15321=DIRECTION('ref_axis',(0.,0.,-1.));
#15322=DIRECTION('center_axis',(0.,0.866025403784438,0.500000000000001));
#15323=DIRECTION('ref_axis',(0.,-0.500000000000001,0.866025403784438));
#15324=DIRECTION('',(-1.,0.,0.));
#15325=DIRECTION('',(0.,0.5,-0.866025403784438));
#15326=DIRECTION('',(0.,0.5,-0.866025403784438));
#15327=DIRECTION('',(-1.,0.,0.));
#15328=DIRECTION('center_axis',(0.,-6.00925839494864E-16,1.));
#15329=DIRECTION('ref_axis',(0.,-1.,-6.00925839494864E-16));
#15330=DIRECTION('',(0.,1.,6.00925839494864E-16));
#15331=DIRECTION('',(0.,1.,6.00925839494864E-16));
#15332=DIRECTION('',(-1.,0.,0.));
#15333=DIRECTION('center_axis',(0.,-0.866025403784438,0.500000000000001));
#15334=DIRECTION('ref_axis',(0.,-0.500000000000001,-0.866025403784438));
#15335=DIRECTION('',(0.,0.5,0.866025403784438));
#15336=DIRECTION('',(0.,0.5,0.866025403784438));
#15337=DIRECTION('',(-1.,0.,0.));
#15338=DIRECTION('center_axis',(0.,-0.866025403784438,-0.5));
#15339=DIRECTION('ref_axis',(0.,0.5,-0.866025403784438));
#15340=DIRECTION('',(0.,-0.5,0.866025403784438));
#15341=DIRECTION('',(0.,-0.5,0.866025403784438));
#15342=DIRECTION('',(-1.,0.,0.));
#15343=DIRECTION('center_axis',(0.,0.,-1.));
#15344=DIRECTION('ref_axis',(-1.,0.,0.));
#15345=DIRECTION('',(0.,-1.,0.));
#15346=DIRECTION('',(0.,-1.,0.));
#15347=DIRECTION('',(-1.,0.,0.));
#15348=DIRECTION('center_axis',(0.,0.866025403784438,-0.500000000000001));
#15349=DIRECTION('ref_axis',(0.,0.500000000000001,0.866025403784438));
#15350=DIRECTION('',(0.,-0.500000000000001,-0.866025403784438));
#15351=DIRECTION('',(0.,-0.500000000000001,-0.866025403784438));
#15352=DIRECTION('center_axis',(-1.,0.,0.));
#15353=DIRECTION('ref_axis',(0.,0.,1.));
#15354=DIRECTION('center_axis',(-1.,0.,0.));
#15355=DIRECTION('ref_axis',(0.,0.,1.));
#15356=DIRECTION('center_axis',(-1.,0.,0.));
#15357=DIRECTION('ref_axis',(0.,0.,1.));
#15358=DIRECTION('center_axis',(-1.,0.,0.));
#15359=DIRECTION('ref_axis',(0.,0.,1.));
#15360=DIRECTION('center_axis',(-1.,0.,0.));
#15361=DIRECTION('ref_axis',(0.,0.,1.));
#15362=DIRECTION('center_axis',(-1.,0.,0.));
#15363=DIRECTION('ref_axis',(0.,0.,1.));
#15364=DIRECTION('',(3.08148791101958E-33,1.,-1.38777878078145E-17));
#15365=DIRECTION('',(4.21687917729221E-81,1.38777878078145E-17,1.));
#15366=DIRECTION('',(-1.22193328862674E-16,1.,1.35112551100538E-16));
#15367=DIRECTION('',(1.,1.22193328862674E-16,-5.55111512312578E-16));
#15368=DIRECTION('',(0.,0.,1.));
#15369=DIRECTION('',(1.,0.,0.));
#15370=DIRECTION('',(-0.559486430143141,-1.15014975916039E-17,-0.828839510692923));
#15371=DIRECTION('',(-0.828839510692923,7.76296027337096E-18,0.559486430143141));
#15372=DIRECTION('',(-0.816414234491854,-5.85498575640092E-17,-0.577466707022214));
#15373=DIRECTION('',(3.04448277876703E-17,-1.,5.83484145176977E-17));
#15374=DIRECTION('',(-0.559486430143122,2.00697438324389E-16,-0.828839510692936));
#15375=DIRECTION('',(0.828839510692936,5.2064852114336E-17,-0.559486430143122));
#15376=DIRECTION('',(-1.,-4.90786712029229E-17,-1.12098963125959E-16));
#15377=DIRECTION('',(-1.12098963125959E-16,7.51498030172846E-17,1.));
#15378=DIRECTION('',(-1.,-4.5595672542045E-17,-2.77555756156289E-17));
#15379=DIRECTION('',(-2.77555756156289E-17,8.7546286988116E-21,1.));
#15380=DIRECTION('',(3.08148791101958E-33,1.,-1.38777878078145E-17));
#15381=DIRECTION('',(4.21687917729221E-81,1.38777878078145E-17,1.));
#15382=DIRECTION('',(3.30393291269521E-18,-1.,1.30289205323433E-17));
#15383=DIRECTION('',(1.,3.30393291269521E-18,5.55111512312578E-17));
#15384=DIRECTION('',(-0.559486430143141,-1.15016104428183E-17,-0.828839510692923));
#15385=DIRECTION('',(0.828839510692923,-7.76389585186165E-18,-0.559486430143141));
#15386=DIRECTION('',(0.435717318662136,1.24912642046109E-17,0.900083561797391));
#15387=DIRECTION('',(-1.1526025521076E-21,1.,-1.38773359784223E-17));
#15388=DIRECTION('',(0.991637787632256,1.7907413119342E-18,0.129052307766292));
#15389=DIRECTION('',(-2.18865530040053E-22,-1.,1.38777707912635E-17));
#15390=DIRECTION('',(0.965943966457478,-3.59110313894971E-18,-0.258751335579925));
#15391=DIRECTION('',(-2.18865530031646E-22,-1.,1.38777707912635E-17));
#15392=DIRECTION('',(-5.84102057453023E-17,-5.84102057453023E-17,1.));
#15393=DIRECTION('',(-2.32681655222893E-18,1.,5.84102057453023E-17));
#15394=DIRECTION('',(-5.84102057453023E-17,-5.84102057453023E-17,1.));
#15395=DIRECTION('',(-2.32681655222893E-18,1.,5.84102057453023E-17));
#15396=DIRECTION('',(-0.559486430143128,-1.27171496124848E-17,-0.828839510692932));
#15397=DIRECTION('',(-0.828839510692932,1.42397759455061E-16,0.559486430143128));
#15398=DIRECTION('',(-0.386307983597981,-1.91009517114284E-16,0.922369850877869));
#15399=DIRECTION('',(-0.922369850877869,3.3637233116923E-17,-0.386307983597981));
#15400=DIRECTION('',(-0.386307983597981,1.28004951514705E-17,0.922369850877869));
#15401=DIRECTION('',(0.922369850877869,5.36110357439148E-18,0.386307983597981));
#15402=DIRECTION('',(-1.,-3.29221414061892E-16,6.93889390390723E-16));
#15403=DIRECTION('',(-6.93889390390723E-16,2.58957848675696E-16,-1.));
#15404=DIRECTION('',(-1.,5.68562149814269E-17,-1.52655665885959E-16));
#15405=DIRECTION('',(1.52655665885959E-16,-3.13372256602295E-17,-1.));
#15406=DIRECTION('',(-0.386307983597981,-2.7310089676497E-17,0.922369850877869));
#15407=DIRECTION('',(0.922369850877869,-2.25809587496626E-16,0.386307983597981));
#15408=DIRECTION('',(-0.386307983597981,-4.912412065024E-16,0.922369850877869));
#15409=DIRECTION('',(-0.922369850877869,3.24654596190217E-16,-0.386307983597981));
#15410=DIRECTION('',(-0.0202499854743108,3.12122153060165E-16,-0.999794948020988));
#15411=DIRECTION('',(-3.88578058618804E-16,1.,3.20056481317721E-16));
#15412=DIRECTION('',(-0.202566335993313,2.34708410590697E-16,-0.979268543108704));
#15413=DIRECTION('',(-3.88578058618804E-16,1.,3.20056481317721E-16));
#15414=DIRECTION('',(-0.135043343595454,2.64649785105168E-16,-0.990839692054451));
#15415=DIRECTION('',(-3.88578058618804E-16,1.,3.20056481317721E-16));
#15416=DIRECTION('',(0.83552699527714,2.63366862315055E-16,-0.549449397272536));
#15417=DIRECTION('',(1.94289029309402E-16,-1.,-1.83880688453542E-16));
#15418=DIRECTION('',(0.83552699527714,2.63366862315055E-16,-0.549449397272536));
#15419=DIRECTION('',(1.94289029309402E-16,-1.,-1.83880688453542E-16));
#15420=DIRECTION('',(0.83552699527714,2.63366862315055E-16,-0.549449397272536));
#15421=DIRECTION('',(1.94289029309402E-16,-1.,-1.83880688453542E-16));
#15422=CARTESIAN_POINT('',(0.,0.,0.));
#15423=CARTESIAN_POINT('',(0.,0.,0.));
#15424=CARTESIAN_POINT('Origin',(7.20000000000006,-20.,9.10000000000001));
#15425=CARTESIAN_POINT('',(7.20000000000006,-20.,7.85000000000001));
#15426=CARTESIAN_POINT('Origin',(7.20000000000006,-20.,9.10000000000001));
#15427=CARTESIAN_POINT('',(7.20000000000006,-17.,7.85000000000001));
#15428=CARTESIAN_POINT('',(7.20000000000006,-20.,7.85000000000001));
#15429=CARTESIAN_POINT('Origin',(7.20000000000006,-17.,9.10000000000001));
#15430=CARTESIAN_POINT('Origin',(7.20000000000006,-20.,9.10000000000001));
#15431=CARTESIAN_POINT('',(7.20000000000006,17.,7.85000000000001));
#15432=CARTESIAN_POINT('Origin',(7.20000000000006,17.,9.10000000000001));
#15433=CARTESIAN_POINT('',(7.20000000000006,20.,7.85000000000001));
#15434=CARTESIAN_POINT('',(7.20000000000006,-20.,7.85000000000001));
#15435=CARTESIAN_POINT('Origin',(7.20000000000006,20.,9.10000000000001));
#15436=CARTESIAN_POINT('Origin',(7.20000000000002,-20.,30.1));
#15437=CARTESIAN_POINT('',(7.20000000000002,-20.,28.85));
#15438=CARTESIAN_POINT('Origin',(7.20000000000002,-20.,30.1));
#15439=CARTESIAN_POINT('',(7.20000000000002,-17.,28.85));
#15440=CARTESIAN_POINT('',(7.20000000000002,-20.,28.85));
#15441=CARTESIAN_POINT('Origin',(7.20000000000002,-17.,30.1));
#15442=CARTESIAN_POINT('Origin',(7.20000000000002,-20.,30.1));
#15443=CARTESIAN_POINT('',(7.20000000000002,17.,28.85));
#15444=CARTESIAN_POINT('Origin',(7.20000000000002,17.,30.1));
#15445=CARTESIAN_POINT('',(7.20000000000002,20.,28.85));
#15446=CARTESIAN_POINT('',(7.20000000000002,-20.,28.85));
#15447=CARTESIAN_POINT('Origin',(7.20000000000002,20.,30.1));
#15448=CARTESIAN_POINT('Origin',(7.2,-20.,58.1));
#15449=CARTESIAN_POINT('',(7.2,-20.,56.85));
#15450=CARTESIAN_POINT('Origin',(7.2,-20.,58.1));
#15451=CARTESIAN_POINT('',(7.2,-17.,56.85));
#15452=CARTESIAN_POINT('',(7.2,-20.,56.85));
#15453=CARTESIAN_POINT('Origin',(7.2,-17.,58.1));
#15454=CARTESIAN_POINT('Origin',(7.2,-20.,58.1));
#15455=CARTESIAN_POINT('',(7.2,17.,56.85));
#15456=CARTESIAN_POINT('Origin',(7.2,17.,58.1));
#15457=CARTESIAN_POINT('',(7.2,20.,56.85));
#15458=CARTESIAN_POINT('',(7.2,-20.,56.85));
#15459=CARTESIAN_POINT('Origin',(7.2,20.,58.1));
#15460=CARTESIAN_POINT('Origin',(7.2,-20.,79.1));
#15461=CARTESIAN_POINT('',(7.2,-20.,77.85));
#15462=CARTESIAN_POINT('Origin',(7.2,-20.,79.1));
#15463=CARTESIAN_POINT('',(7.2,-17.,77.85));
#15464=CARTESIAN_POINT('',(7.2,-20.,77.85));
#15465=CARTESIAN_POINT('Origin',(7.2,-17.,79.1));
#15466=CARTESIAN_POINT('Origin',(7.2,-20.,79.1));
#15467=CARTESIAN_POINT('',(7.2,17.,77.85));
#15468=CARTESIAN_POINT('Origin',(7.2,17.,79.1));
#15469=CARTESIAN_POINT('',(7.2,20.,77.85));
#15470=CARTESIAN_POINT('',(7.2,-20.,77.85));
#15471=CARTESIAN_POINT('Origin',(7.2,20.,79.1));
#15472=CARTESIAN_POINT('Origin',(10.,7.77817459305203,36.321825406948));
#15473=CARTESIAN_POINT('',(0.,9.02817459305202,36.321825406948));
#15474=CARTESIAN_POINT('Origin',(0.,7.77817459305203,36.321825406948));
#15475=CARTESIAN_POINT('',(-3.,9.02817459305202,36.321825406948));
#15476=CARTESIAN_POINT('',(10.,9.02817459305203,36.321825406948));
#15477=CARTESIAN_POINT('Origin',(-3.,7.77817459305203,36.321825406948));
#15478=CARTESIAN_POINT('Origin',(10.,1.70997563773818E-14,33.1));
#15479=CARTESIAN_POINT('',(0.,1.25000000000001,33.1));
#15480=CARTESIAN_POINT('Origin',(0.,1.38777878078145E-14,33.1));
#15481=CARTESIAN_POINT('',(-3.,1.25000000000001,33.1));
#15482=CARTESIAN_POINT('',(10.,1.25000000000001,33.1));
#15483=CARTESIAN_POINT('Origin',(-3.,1.29111972369443E-14,33.1));
#15484=CARTESIAN_POINT('Origin',(10.,-7.778174593052,36.321825406948));
#15485=CARTESIAN_POINT('',(0.,-6.52817459305201,36.321825406948));
#15486=CARTESIAN_POINT('Origin',(0.,-7.77817459305201,36.321825406948));
#15487=CARTESIAN_POINT('',(-3.,-6.52817459305201,36.321825406948));
#15488=CARTESIAN_POINT('',(10.,-6.52817459305201,36.321825406948));
#15489=CARTESIAN_POINT('Origin',(-3.,-7.77817459305201,36.321825406948));
#15490=CARTESIAN_POINT('Origin',(10.,-11.,44.1));
#15491=CARTESIAN_POINT('',(0.,-9.74999999999998,44.1));
#15492=CARTESIAN_POINT('Origin',(0.,-11.,44.1));
#15493=CARTESIAN_POINT('',(-3.,-9.74999999999998,44.1));
#15494=CARTESIAN_POINT('',(10.,-9.74999999999998,44.1));
#15495=CARTESIAN_POINT('Origin',(-3.,-11.,44.1));
#15496=CARTESIAN_POINT('Origin',(10.,-7.778174593052,51.878174593052));
#15497=CARTESIAN_POINT('',(0.,-6.52817459305201,51.878174593052));
#15498=CARTESIAN_POINT('Origin',(0.,-7.77817459305201,51.878174593052));
#15499=CARTESIAN_POINT('',(-3.,-6.52817459305201,51.878174593052));
#15500=CARTESIAN_POINT('',(10.,-6.52817459305201,51.878174593052));
#15501=CARTESIAN_POINT('Origin',(-3.,-7.77817459305201,51.878174593052));
#15502=CARTESIAN_POINT('Origin',(10.,1.79671181153702E-14,55.1));
#15503=CARTESIAN_POINT('',(0.,1.25000000000001,55.1));
#15504=CARTESIAN_POINT('Origin',(0.,1.47451495458029E-14,55.1));
#15505=CARTESIAN_POINT('',(-3.,1.25000000000001,55.1));
#15506=CARTESIAN_POINT('',(10.,1.25000000000002,55.1));
#15507=CARTESIAN_POINT('Origin',(-3.,1.37785589749327E-14,55.1));
#15508=CARTESIAN_POINT('Origin',(10.,7.77817459305203,51.878174593052));
#15509=CARTESIAN_POINT('',(0.,9.02817459305204,51.878174593052));
#15510=CARTESIAN_POINT('Origin',(0.,7.77817459305203,51.878174593052));
#15511=CARTESIAN_POINT('',(-3.,9.02817459305203,51.878174593052));
#15512=CARTESIAN_POINT('',(10.,9.02817459305204,51.878174593052));
#15513=CARTESIAN_POINT('Origin',(-3.,7.77817459305203,51.878174593052));
#15514=CARTESIAN_POINT('Origin',(10.,11.,44.1));
#15515=CARTESIAN_POINT('',(0.,12.25,44.1));
#15516=CARTESIAN_POINT('Origin',(0.,11.,44.1));
#15517=CARTESIAN_POINT('',(-3.,12.25,44.1));
#15518=CARTESIAN_POINT('',(10.,12.25,44.1));
#15519=CARTESIAN_POINT('Origin',(-3.,11.,44.1));
#15520=CARTESIAN_POINT('Origin',(10.,4.95669204554415E-15,44.1));
#15521=CARTESIAN_POINT('',(0.,5.,44.1));
#15522=CARTESIAN_POINT('Origin',(0.,1.73472347597681E-15,44.1));
#15523=CARTESIAN_POINT('',(-3.,5.,44.1));
#15524=CARTESIAN_POINT('',(10.,5.,44.1));
#15525=CARTESIAN_POINT('Origin',(-3.,7.68132905106604E-16,44.1));
#15526=CARTESIAN_POINT('Origin',(0.,14.,88.2));
#15527=CARTESIAN_POINT('',(0.,14.,88.2));
#15528=CARTESIAN_POINT('',(-3.,14.,88.2));
#15529=CARTESIAN_POINT('',(0.,14.,88.2));
#15530=CARTESIAN_POINT('',(3.,17.,88.2));
#15531=CARTESIAN_POINT('Origin',(3.,14.,88.2));
#15532=CARTESIAN_POINT('',(3.,20.,88.2));
#15533=CARTESIAN_POINT('',(3.,20.,88.2));
#15534=CARTESIAN_POINT('Origin',(3.,14.,88.2));
#15535=CARTESIAN_POINT('Origin',(3.,20.,88.2));
#15536=CARTESIAN_POINT('',(4.51075599739428E-15,-14.,88.2));
#15537=CARTESIAN_POINT('',(0.,0.,88.2));
#15538=CARTESIAN_POINT('',(-3.,-14.,88.2));
#15539=CARTESIAN_POINT('',(-3.,0.,88.2));
#15540=CARTESIAN_POINT('',(-3.,-14.,88.2));
#15541=CARTESIAN_POINT('Origin',(3.,17.,0.));
#15542=CARTESIAN_POINT('',(3.,17.,0.));
#15543=CARTESIAN_POINT('',(3.,20.,0.));
#15544=CARTESIAN_POINT('',(3.,17.,0.));
#15545=CARTESIAN_POINT('',(0.,14.,0.));
#15546=CARTESIAN_POINT('Origin',(3.,14.,0.));
#15547=CARTESIAN_POINT('',(-3.,14.,0.));
#15548=CARTESIAN_POINT('',(-3.,14.,0.));
#15549=CARTESIAN_POINT('Origin',(3.,14.,0.));
#15550=CARTESIAN_POINT('Origin',(-3.,14.,0.));
#15551=CARTESIAN_POINT('',(3.96446609406726,20.,0.));
#15552=CARTESIAN_POINT('',(0.,20.,0.));
#15553=CARTESIAN_POINT('',(3.96446609406726,17.,0.));
#15554=CARTESIAN_POINT('',(3.96446609406726,14.,0.));
#15555=CARTESIAN_POINT('',(0.,17.,0.));
#15556=CARTESIAN_POINT('Origin',(3.,-17.,88.2));
#15557=CARTESIAN_POINT('',(3.,-17.,88.2));
#15558=CARTESIAN_POINT('',(3.,-20.,88.2));
#15559=CARTESIAN_POINT('',(3.,-17.,88.2));
#15560=CARTESIAN_POINT('Origin',(3.,-14.,88.2));
#15561=CARTESIAN_POINT('Origin',(3.,-14.,88.2));
#15562=CARTESIAN_POINT('Origin',(-3.,-14.,88.2));
#15563=CARTESIAN_POINT('',(3.96446609406726,-20.,88.2));
#15564=CARTESIAN_POINT('',(5.47734656826449E-15,-20.,88.2));
#15565=CARTESIAN_POINT('',(3.96446609406726,-17.,88.2));
#15566=CARTESIAN_POINT('',(3.96446609406726,-14.,88.2));
#15567=CARTESIAN_POINT('',(5.47734656826449E-15,-17.,88.2));
#15568=CARTESIAN_POINT('Origin',(4.51075599739428E-15,-14.,0.));
#15569=CARTESIAN_POINT('',(4.51075599739428E-15,-14.,0.));
#15570=CARTESIAN_POINT('',(-3.,-14.,0.));
#15571=CARTESIAN_POINT('',(4.51075599739428E-15,-14.,0.));
#15572=CARTESIAN_POINT('',(3.,-17.,0.));
#15573=CARTESIAN_POINT('Origin',(3.,-14.,0.));
#15574=CARTESIAN_POINT('',(3.,-20.,0.));
#15575=CARTESIAN_POINT('',(3.,-20.,0.));
#15576=CARTESIAN_POINT('Origin',(3.,-14.,0.));
#15577=CARTESIAN_POINT('Origin',(3.,-20.,0.));
#15578=CARTESIAN_POINT('',(0.,0.,0.));
#15579=CARTESIAN_POINT('',(-3.,-9.66590570870203E-16,0.));
#15580=CARTESIAN_POINT('Origin',(5.47734656826449E-15,-20.,88.2));
#15581=CARTESIAN_POINT('',(9.26776695296637,-20.,83.9322330470336));
#15582=CARTESIAN_POINT('',(5.73223304703362,-20.,87.4677669529664));
#15583=CARTESIAN_POINT('',(10.,-20.,83.2));
#15584=CARTESIAN_POINT('Origin',(3.96446609406726,-20.,85.7));
#15585=CARTESIAN_POINT('',(3.,-20.,88.2));
#15586=CARTESIAN_POINT('',(3.96446609406726,-20.,0.));
#15587=CARTESIAN_POINT('',(5.47734656826449E-15,-20.,0.));
#15588=CARTESIAN_POINT('',(5.73223304703363,-20.,0.732233047033637));
#15589=CARTESIAN_POINT('Origin',(3.96446609406726,-20.,2.5));
#15590=CARTESIAN_POINT('',(9.26776695296638,-20.,4.2677669529664));
#15591=CARTESIAN_POINT('',(5.,-20.,0.));
#15592=CARTESIAN_POINT('',(10.,-20.,6.03553390593277));
#15593=CARTESIAN_POINT('Origin',(7.5,-20.,6.03553390593277));
#15594=CARTESIAN_POINT('',(10.,-20.,82.1644660940673));
#15595=CARTESIAN_POINT('',(10.,-20.,88.2));
#15596=CARTESIAN_POINT('Origin',(7.5,-20.,82.1644660940673));
#15597=CARTESIAN_POINT('Origin',(10.,-17.,88.2));
#15598=CARTESIAN_POINT('',(10.,-17.,82.1644660940673));
#15599=CARTESIAN_POINT('',(10.,-17.,6.03553390593277));
#15600=CARTESIAN_POINT('',(10.,-17.,88.2));
#15601=CARTESIAN_POINT('',(10.,-17.,82.1644660940673));
#15602=CARTESIAN_POINT('',(10.,-17.,6.03553390593277));
#15603=CARTESIAN_POINT('Origin',(5.47734656826449E-15,-17.,88.2));
#15604=CARTESIAN_POINT('',(5.73223304703363,-17.,87.4677669529664));
#15605=CARTESIAN_POINT('Origin',(3.96446609406726,-17.,85.7));
#15606=CARTESIAN_POINT('',(9.26776695296638,-17.,83.9322330470336));
#15607=CARTESIAN_POINT('',(2.49999999999999,-17.,90.7));
#15608=CARTESIAN_POINT('Origin',(7.5,-17.,82.1644660940673));
#15609=CARTESIAN_POINT('',(9.26776695296638,-17.,4.2677669529664));
#15610=CARTESIAN_POINT('Origin',(7.5,-17.,6.03553390593277));
#15611=CARTESIAN_POINT('',(5.73223304703364,-17.,0.73223304703364));
#15612=CARTESIAN_POINT('',(46.6,-17.,41.6000000000003));
#15613=CARTESIAN_POINT('',(3.96446609406726,-17.,0.));
#15614=CARTESIAN_POINT('Origin',(3.96446609406726,-17.,2.5));
#15615=CARTESIAN_POINT('',(5.47734656826449E-15,-17.,0.));
#15616=CARTESIAN_POINT('',(3.,-17.,88.2));
#15617=CARTESIAN_POINT('Origin',(3.,-14.,88.2));
#15618=CARTESIAN_POINT('',(4.51075599739428E-15,-14.,88.2));
#15619=CARTESIAN_POINT('Origin',(0.,0.,88.2));
#15620=CARTESIAN_POINT('',(0.,14.,88.2));
#15621=CARTESIAN_POINT('Origin',(3.,14.,88.2));
#15622=CARTESIAN_POINT('',(3.,17.,88.2));
#15623=CARTESIAN_POINT('Origin',(0.,17.,88.2));
#15624=CARTESIAN_POINT('',(5.73223304703363,17.,0.732233047033647));
#15625=CARTESIAN_POINT('Origin',(3.96446609406726,17.,2.5));
#15626=CARTESIAN_POINT('',(9.26776695296638,17.,4.26776695296641));
#15627=CARTESIAN_POINT('',(46.6,17.,41.6000000000003));
#15628=CARTESIAN_POINT('',(10.,17.,6.03553390593277));
#15629=CARTESIAN_POINT('Origin',(7.5,17.,6.03553390593277));
#15630=CARTESIAN_POINT('',(10.,17.,82.1644660940673));
#15631=CARTESIAN_POINT('',(10.,17.,88.2));
#15632=CARTESIAN_POINT('',(9.26776695296637,17.,83.9322330470337));
#15633=CARTESIAN_POINT('Origin',(7.5,17.,82.1644660940673));
#15634=CARTESIAN_POINT('',(5.73223304703364,17.,87.4677669529664));
#15635=CARTESIAN_POINT('',(2.5,17.,90.7));
#15636=CARTESIAN_POINT('',(3.96446609406727,17.,88.2));
#15637=CARTESIAN_POINT('Origin',(3.96446609406727,17.,85.7));
#15638=CARTESIAN_POINT('',(0.,17.,88.2));
#15639=CARTESIAN_POINT('Origin',(10.,20.,88.2));
#15640=CARTESIAN_POINT('',(10.,20.,6.03553390593277));
#15641=CARTESIAN_POINT('',(10.,20.,6.03553390593277));
#15642=CARTESIAN_POINT('',(10.,20.,82.1644660940673));
#15643=CARTESIAN_POINT('',(10.,20.,88.2));
#15644=CARTESIAN_POINT('',(10.,20.,82.1644660940673));
#15645=CARTESIAN_POINT('Origin',(0.,20.,88.2));
#15646=CARTESIAN_POINT('',(9.26776695296638,20.,4.2677669529664));
#15647=CARTESIAN_POINT('',(5.73223304703363,20.,0.732233047033636));
#15648=CARTESIAN_POINT('',(5.,20.,0.));
#15649=CARTESIAN_POINT('Origin',(3.96446609406726,20.,2.5));
#15650=CARTESIAN_POINT('',(3.,20.,88.2));
#15651=CARTESIAN_POINT('',(3.96446609406727,20.,88.2));
#15652=CARTESIAN_POINT('',(0.,20.,88.2));
#15653=CARTESIAN_POINT('',(5.73223304703364,20.,87.4677669529664));
#15654=CARTESIAN_POINT('Origin',(3.96446609406727,20.,85.7));
#15655=CARTESIAN_POINT('',(9.26776695296637,20.,83.9322330470337));
#15656=CARTESIAN_POINT('',(10.,20.,83.2));
#15657=CARTESIAN_POINT('Origin',(7.5,20.,82.1644660940673));
#15658=CARTESIAN_POINT('Origin',(7.5,20.,6.03553390593277));
#15659=CARTESIAN_POINT('Origin',(3.,14.,88.2));
#15660=CARTESIAN_POINT('',(-3.,14.,88.2));
#15661=CARTESIAN_POINT('Origin',(-3.,-9.66590570870203E-16,88.2));
#15662=CARTESIAN_POINT('',(-3.,-14.,88.2));
#15663=CARTESIAN_POINT('Origin',(3.,-14.,88.2));
#15664=CARTESIAN_POINT('Origin',(3.,-14.,88.2));
#15665=CARTESIAN_POINT('',(3.96446609406727,20.,88.2));
#15666=CARTESIAN_POINT('Origin',(3.,-14.,0.));
#15667=CARTESIAN_POINT('',(3.96446609406726,-14.,0.));
#15668=CARTESIAN_POINT('Origin',(5.,-14.,0.));
#15669=CARTESIAN_POINT('',(9.26776695296638,-14.,4.2677669529664));
#15670=CARTESIAN_POINT('',(5.73223304703363,-14.,0.732233047033636));
#15671=CARTESIAN_POINT('Origin',(5.,14.,0.));
#15672=CARTESIAN_POINT('',(5.73223304703363,14.,0.732233047033636));
#15673=CARTESIAN_POINT('',(9.26776695296638,14.,4.2677669529664));
#15674=CARTESIAN_POINT('Origin',(10.,-17.,83.2));
#15675=CARTESIAN_POINT('',(5.73223304703363,-17.,87.4677669529664));
#15676=CARTESIAN_POINT('',(9.26776695296637,-17.,83.9322330470336));
#15677=CARTESIAN_POINT('Origin',(10.,20.,83.2));
#15678=CARTESIAN_POINT('',(5.73223304703364,17.,87.4677669529664));
#15679=CARTESIAN_POINT('',(9.26776695296637,20.,83.9322330470337));
#15680=CARTESIAN_POINT('Origin',(3.96446609406726,-14.,85.7));
#15681=CARTESIAN_POINT('Origin',(7.5,-17.,82.1644660940673));
#15682=CARTESIAN_POINT('Origin',(7.5,-17.,6.03553390593277));
#15683=CARTESIAN_POINT('Origin',(3.96446609406726,-14.,2.5));
#15684=CARTESIAN_POINT('Origin',(3.96446609406726,14.,2.5));
#15685=CARTESIAN_POINT('Origin',(7.5,20.,6.03553390593277));
#15686=CARTESIAN_POINT('Origin',(3.96446609406727,-14.,85.7));
#15687=CARTESIAN_POINT('Origin',(7.5,20.,82.1644660940673));
#15688=CARTESIAN_POINT('',(0.,0.,0.));
#15689=CARTESIAN_POINT('Origin',(0.,0.,-1.05));
#15690=CARTESIAN_POINT('',(-5.5,-6.73555739531044E-16,21.));
#15691=CARTESIAN_POINT('Origin',(0.,0.,21.));
#15692=CARTESIAN_POINT('',(-5.5,-6.73555739531044E-16,20.5));
#15693=CARTESIAN_POINT('',(-5.5,-6.73555739531044E-16,-1.05));
#15694=CARTESIAN_POINT('Origin',(0.,0.,20.5));
#15695=CARTESIAN_POINT('Origin',(0.,0.,28.375));
#15696=CARTESIAN_POINT('',(14.,-1.71450551880629E-15,21.));
#15697=CARTESIAN_POINT('Origin',(0.,0.,21.));
#15698=CARTESIAN_POINT('',(14.,-1.71450551880629E-15,23.5));
#15699=CARTESIAN_POINT('',(14.,-1.71450551880629E-15,28.375));
#15700=CARTESIAN_POINT('Origin',(0.,0.,23.5));
#15701=CARTESIAN_POINT('Origin',(11.,-45.3,0.));
#15702=CARTESIAN_POINT('',(12.35,-45.3,-14.5));
#15703=CARTESIAN_POINT('Origin',(11.,-45.3,-14.5));
#15704=CARTESIAN_POINT('',(12.35,-45.3,-17.));
#15705=CARTESIAN_POINT('',(12.35,-45.3,0.));
#15706=CARTESIAN_POINT('Origin',(11.,-45.3,-17.));
#15707=CARTESIAN_POINT('Origin',(17.3,-18.,0.));
#15708=CARTESIAN_POINT('',(18.65,-18.,-14.5));
#15709=CARTESIAN_POINT('Origin',(17.3,-18.,-14.5));
#15710=CARTESIAN_POINT('',(18.65,-18.,-17.));
#15711=CARTESIAN_POINT('',(18.65,-18.,0.));
#15712=CARTESIAN_POINT('Origin',(17.3,-18.,-17.));
#15713=CARTESIAN_POINT('Origin',(17.3,4.,0.));
#15714=CARTESIAN_POINT('',(18.65,4.,-14.5));
#15715=CARTESIAN_POINT('Origin',(17.3,4.,-14.5));
#15716=CARTESIAN_POINT('',(18.65,4.,-17.));
#15717=CARTESIAN_POINT('',(18.65,4.,0.));
#15718=CARTESIAN_POINT('Origin',(17.3,4.,-17.));
#15719=CARTESIAN_POINT('Origin',(-11.,-45.3,0.));
#15720=CARTESIAN_POINT('',(-9.65,-45.3,-14.5));
#15721=CARTESIAN_POINT('Origin',(-11.,-45.3,-14.5));
#15722=CARTESIAN_POINT('',(-9.65,-45.3,-17.));
#15723=CARTESIAN_POINT('',(-9.65,-45.3,0.));
#15724=CARTESIAN_POINT('Origin',(-11.,-45.3,-17.));
#15725=CARTESIAN_POINT('Origin',(-17.3,-18.,0.));
#15726=CARTESIAN_POINT('',(-15.95,-18.,-14.5));
#15727=CARTESIAN_POINT('Origin',(-17.3,-18.,-14.5));
#15728=CARTESIAN_POINT('',(-15.95,-18.,-17.));
#15729=CARTESIAN_POINT('',(-15.95,-18.,0.));
#15730=CARTESIAN_POINT('Origin',(-17.3,-18.,-17.));
#15731=CARTESIAN_POINT('Origin',(-17.3,4.,0.));
#15732=CARTESIAN_POINT('',(-15.95,4.,-14.5));
#15733=CARTESIAN_POINT('Origin',(-17.3,4.,-14.5));
#15734=CARTESIAN_POINT('',(-15.95,4.,-17.));
#15735=CARTESIAN_POINT('',(-15.95,4.,0.));
#15736=CARTESIAN_POINT('Origin',(-17.3,4.,-17.));
#15737=CARTESIAN_POINT('Origin',(11.,-45.3,0.));
#15738=CARTESIAN_POINT('',(12.35,-45.3,17.));
#15739=CARTESIAN_POINT('Origin',(11.,-45.3,17.));
#15740=CARTESIAN_POINT('',(12.35,-45.3,14.5));
#15741=CARTESIAN_POINT('',(12.35,-45.3,0.));
#15742=CARTESIAN_POINT('Origin',(11.,-45.3,14.5));
#15743=CARTESIAN_POINT('Origin',(17.3,-18.,0.));
#15744=CARTESIAN_POINT('',(18.65,-18.,17.));
#15745=CARTESIAN_POINT('Origin',(17.3,-18.,17.));
#15746=CARTESIAN_POINT('',(18.65,-18.,14.5));
#15747=CARTESIAN_POINT('',(18.65,-18.,0.));
#15748=CARTESIAN_POINT('Origin',(17.3,-18.,14.5));
#15749=CARTESIAN_POINT('Origin',(17.3,4.,0.));
#15750=CARTESIAN_POINT('',(18.65,4.,17.));
#15751=CARTESIAN_POINT('Origin',(17.3,4.,17.));
#15752=CARTESIAN_POINT('',(18.65,4.,14.5));
#15753=CARTESIAN_POINT('',(18.65,4.,0.));
#15754=CARTESIAN_POINT('Origin',(17.3,4.,14.5));
#15755=CARTESIAN_POINT('Origin',(-11.,-45.3,0.));
#15756=CARTESIAN_POINT('',(-9.65,-45.3,17.));
#15757=CARTESIAN_POINT('Origin',(-11.,-45.3,17.));
#15758=CARTESIAN_POINT('',(-9.65,-45.3,14.5));
#15759=CARTESIAN_POINT('',(-9.65,-45.3,0.));
#15760=CARTESIAN_POINT('Origin',(-11.,-45.3,14.5));
#15761=CARTESIAN_POINT('Origin',(-17.3,-18.,0.));
#15762=CARTESIAN_POINT('',(-15.95,-18.,17.));
#15763=CARTESIAN_POINT('Origin',(-17.3,-18.,17.));
#15764=CARTESIAN_POINT('',(-15.95,-18.,14.5));
#15765=CARTESIAN_POINT('',(-15.95,-18.,0.));
#15766=CARTESIAN_POINT('Origin',(-17.3,-18.,14.5));
#15767=CARTESIAN_POINT('Origin',(-17.3,4.,0.));
#15768=CARTESIAN_POINT('',(-15.95,4.,17.));
#15769=CARTESIAN_POINT('Origin',(-17.3,4.,17.));
#15770=CARTESIAN_POINT('',(-15.95,4.,14.5));
#15771=CARTESIAN_POINT('',(-15.95,4.,0.));
#15772=CARTESIAN_POINT('Origin',(-17.3,4.,14.5));
#15773=CARTESIAN_POINT('Origin',(0.,0.,28.375));
#15774=CARTESIAN_POINT('',(5.,-6.12323399573677E-16,23.5));
#15775=CARTESIAN_POINT('Origin',(0.,0.,23.5));
#15776=CARTESIAN_POINT('',(5.,-6.12323399573677E-16,25.));
#15777=CARTESIAN_POINT('',(5.,-6.12323399573677E-16,28.375));
#15778=CARTESIAN_POINT('Origin',(0.,0.,25.));
#15779=CARTESIAN_POINT('Origin',(0.,0.,-23.1));
#15780=CARTESIAN_POINT('',(-7.5,-9.18485099360515E-16,-20.5));
#15781=CARTESIAN_POINT('Origin',(0.,0.,-20.5));
#15782=CARTESIAN_POINT('',(-7.5,-9.18485099360515E-16,-19.5));
#15783=CARTESIAN_POINT('',(-7.5,-9.18485099360515E-16,-23.1));
#15784=CARTESIAN_POINT('Origin',(0.,0.,-19.5));
#15785=CARTESIAN_POINT('Origin',(0.,0.,28.375));
#15786=CARTESIAN_POINT('',(2.75,-3.36777869765522E-16,25.));
#15787=CARTESIAN_POINT('Origin',(0.,0.,25.));
#15788=CARTESIAN_POINT('',(2.75,-3.36777869765522E-16,28.));
#15789=CARTESIAN_POINT('',(2.75,-3.36777869765522E-16,28.375));
#15790=CARTESIAN_POINT('Origin',(0.,0.,28.));
#15791=CARTESIAN_POINT('Origin',(0.,0.,-23.1));
#15792=CARTESIAN_POINT('',(-5.,-6.12323399573677E-16,-19.5));
#15793=CARTESIAN_POINT('Origin',(0.,0.,-19.5));
#15794=CARTESIAN_POINT('',(-5.,-6.12323399573677E-16,-19.8));
#15795=CARTESIAN_POINT('',(-5.,-6.12323399573677E-16,-23.1));
#15796=CARTESIAN_POINT('Origin',(0.,0.,-19.8));
#15797=CARTESIAN_POINT('Origin',(0.,0.,1.305));
#15798=CARTESIAN_POINT('',(7.25,-8.87868929381831E-16,-21.));
#15799=CARTESIAN_POINT('Origin',(0.,0.,-21.));
#15800=CARTESIAN_POINT('',(7.25,-8.87868929381831E-16,-19.8));
#15801=CARTESIAN_POINT('',(7.25,-8.87868929381831E-16,1.305));
#15802=CARTESIAN_POINT('Origin',(0.,0.,-19.8));
#15803=CARTESIAN_POINT('Origin',(0.,0.,1.305));
#15804=CARTESIAN_POINT('',(14.,-1.71450551880629E-15,-23.5));
#15805=CARTESIAN_POINT('Origin',(0.,0.,-23.5));
#15806=CARTESIAN_POINT('',(14.,-1.71450551880629E-15,-21.));
#15807=CARTESIAN_POINT('',(14.,-1.71450551880629E-15,1.305));
#15808=CARTESIAN_POINT('Origin',(0.,0.,-21.));
#15809=CARTESIAN_POINT('Origin',(0.,0.,1.305));
#15810=CARTESIAN_POINT('',(4.75,-5.81707229594993E-16,-24.3));
#15811=CARTESIAN_POINT('Origin',(0.,0.,-24.3));
#15812=CARTESIAN_POINT('',(4.75,-5.81707229594993E-16,-23.5));
#15813=CARTESIAN_POINT('',(4.75,-5.81707229594993E-16,1.305));
#15814=CARTESIAN_POINT('Origin',(0.,0.,-23.5));
#15815=CARTESIAN_POINT('Origin',(0.,0.,1.305));
#15816=CARTESIAN_POINT('',(2.75,-3.36777869765522E-16,-26.1));
#15817=CARTESIAN_POINT('Origin',(0.,0.,-26.1));
#15818=CARTESIAN_POINT('',(2.75,-3.36777869765522E-16,-24.3));
#15819=CARTESIAN_POINT('',(2.75,-3.36777869765522E-16,1.305));
#15820=CARTESIAN_POINT('Origin',(0.,0.,-24.3));
#15821=CARTESIAN_POINT('Origin',(0.,0.,20.5));
#15822=CARTESIAN_POINT('',(13.,-41.,20.5));
#15823=CARTESIAN_POINT('',(13.0000000000055,11.,20.4999999999987));
#15824=CARTESIAN_POINT('',(13.,0.,20.5));
#15825=CARTESIAN_POINT('',(-13.,10.9999999999864,20.4999999999983));
#15826=CARTESIAN_POINT('',(0.,11.,20.5));
#15827=CARTESIAN_POINT('',(-13.,-41.,20.5));
#15828=CARTESIAN_POINT('',(-13.,0.,20.5));
#15829=CARTESIAN_POINT('',(0.,-41.,20.5));
#15830=CARTESIAN_POINT('Origin',(14.63200966641,11.,18.5));
#15831=CARTESIAN_POINT('',(13.,12.9999999999984,18.4999999991966));
#15832=CARTESIAN_POINT('Origin',(13.,11.,18.5));
#15833=CARTESIAN_POINT('',(-12.9999999999935,13.0000000000008,18.49999999892));
#15834=CARTESIAN_POINT('',(14.63200966641,13.,18.49999999892));
#15835=CARTESIAN_POINT('Origin',(-13.,11.,18.5));
#15836=CARTESIAN_POINT('Origin',(13.,-42.63464535978,19.));
#15837=CARTESIAN_POINT('',(14.5000000000004,-41.,18.9999999999984));
#15838=CARTESIAN_POINT('',(14.5000000000014,11.0000000000001,18.999999864659));
#15839=CARTESIAN_POINT('',(14.5,-42.63464535978,19.));
#15840=CARTESIAN_POINT('Origin',(13.,11.,19.));
#15841=CARTESIAN_POINT('Origin',(13.,-41.,19.));
#15842=CARTESIAN_POINT('Origin',(-14.67485779376,-41.,19.));
#15843=CARTESIAN_POINT('',(-13.,-42.5000000000004,18.9999999999985));
#15844=CARTESIAN_POINT('',(13.,-42.5000000000002,19.));
#15845=CARTESIAN_POINT('',(-14.67485779376,-42.5,19.));
#15846=CARTESIAN_POINT('Origin',(13.,-41.,19.));
#15847=CARTESIAN_POINT('Origin',(-13.,-41.,19.));
#15848=CARTESIAN_POINT('Origin',(-13.,11.13971317669,19.));
#15849=CARTESIAN_POINT('',(-14.5000000000014,11.000000000002,18.9999998643683));
#15850=CARTESIAN_POINT('Origin',(-13.,11.,19.));
#15851=CARTESIAN_POINT('',(-14.5000000000002,-41.0000000021332,18.9999998796623));
#15852=CARTESIAN_POINT('',(-14.5,11.13971317669,18.99999972876));
#15853=CARTESIAN_POINT('Origin',(-13.,-41.,19.));
#15854=CARTESIAN_POINT('Origin',(0.,0.,21.));
#15855=CARTESIAN_POINT('Origin',(14.5,13.,-20.5));
#15856=CARTESIAN_POINT('',(13.,13.,17.));
#15857=CARTESIAN_POINT('',(13.,13.,18.63971317669));
#15858=CARTESIAN_POINT('',(13.94140536675,13.,17.));
#15859=CARTESIAN_POINT('',(0.,13.,17.));
#15860=CARTESIAN_POINT('',(13.94140536675,13.,14.5));
#15861=CARTESIAN_POINT('',(13.94140536675,13.,-20.5));
#15862=CARTESIAN_POINT('',(12.5,13.,14.5));
#15863=CARTESIAN_POINT('',(0.,13.,14.5));
#15864=CARTESIAN_POINT('',(12.5,13.,-14.5));
#15865=CARTESIAN_POINT('',(12.5,13.,-20.5));
#15866=CARTESIAN_POINT('',(13.94140536675,13.,-14.5));
#15867=CARTESIAN_POINT('',(0.,13.,-14.5));
#15868=CARTESIAN_POINT('',(13.94140536675,13.,-17.));
#15869=CARTESIAN_POINT('',(13.94140536675,13.,-20.5));
#15870=CARTESIAN_POINT('',(6.65,13.,-17.));
#15871=CARTESIAN_POINT('',(14.5,13.,-17.));
#15872=CARTESIAN_POINT('',(-6.65,13.,-17.));
#15873=CARTESIAN_POINT('',(14.5,13.,-17.));
#15874=CARTESIAN_POINT('',(-13.94140536675,13.,-17.));
#15875=CARTESIAN_POINT('',(14.5,13.,-17.));
#15876=CARTESIAN_POINT('',(-13.94140536675,13.,-14.5));
#15877=CARTESIAN_POINT('',(-13.94140536675,13.,-20.5));
#15878=CARTESIAN_POINT('',(-12.5,13.,-14.5));
#15879=CARTESIAN_POINT('',(0.,13.,-14.5));
#15880=CARTESIAN_POINT('',(-12.5,13.,14.5));
#15881=CARTESIAN_POINT('',(-12.5,13.,-20.5));
#15882=CARTESIAN_POINT('',(-13.94140536675,13.,14.5));
#15883=CARTESIAN_POINT('',(0.,13.,14.5));
#15884=CARTESIAN_POINT('',(-13.94140536675,13.,17.));
#15885=CARTESIAN_POINT('',(-13.94140536675,13.,-20.5));
#15886=CARTESIAN_POINT('',(-13.,13.,17.));
#15887=CARTESIAN_POINT('',(0.,13.,17.));
#15888=CARTESIAN_POINT('',(-13.,13.,-17.13464535978));
#15889=CARTESIAN_POINT('Ctrl Pts',(14.5000000000041,11.0000000000019,18.99999972876));
#15890=CARTESIAN_POINT('Ctrl Pts',(14.5000000000077,11.499999728971,18.9999997287616));
#15891=CARTESIAN_POINT('Ctrl Pts',(14.5000000000013,11.4999997287644,18.4999999997925));
#15892=CARTESIAN_POINT('Ctrl Pts',(14.5000001123536,11.0000000000019,19.6213201517653));
#15893=CARTESIAN_POINT('Ctrl Pts',(14.5000001123618,12.1213201522332,19.621320151769));
#15894=CARTESIAN_POINT('Ctrl Pts',(14.5000001123474,12.1213201517697,18.4999999995377));
#15895=CARTESIAN_POINT('Ctrl Pts',(14.0606602676774,11.0000000000052,20.0606600758827));
#15896=CARTESIAN_POINT('Ctrl Pts',(14.0606602676888,12.5606600765297,20.0606600758878));
#15897=CARTESIAN_POINT('Ctrl Pts',(14.0606602676688,12.5606600758847,18.4999999993632));
#15898=CARTESIAN_POINT('Ctrl Pts',(13.6213204230012,11.0000000000084,20.5000000000001));
#15899=CARTESIAN_POINT('Ctrl Pts',(13.6213204230159,13.0000000008263,20.5000000000066));
#15900=CARTESIAN_POINT('Ctrl Pts',(13.6213204229902,12.9999999999996,18.4999999991887));
#15901=CARTESIAN_POINT('Ctrl Pts',(12.9999999999959,11.0000000000129,20.4999999999974));
#15902=CARTESIAN_POINT('Ctrl Pts',(13.0000000000105,13.0000000008201,20.5000000000039));
#15903=CARTESIAN_POINT('Ctrl Pts',(12.9999999999848,12.9999999999935,18.4999999991966));
#15904=CARTESIAN_POINT('',(14.5000000000009,11.4999998646612,18.4999999999998));
#15905=CARTESIAN_POINT('Origin',(14.4999999999976,11.0000000000019,18.4999999999976));
#15906=CARTESIAN_POINT('Origin',(12.9999999999996,11.4999999999918,18.5000000000193));
#15907=CARTESIAN_POINT('Ctrl Pts',(-13.,10.9999999999728,20.4999999999966));
#15908=CARTESIAN_POINT('Ctrl Pts',(-12.9999999999873,13.000000001073,20.5000000000202));
#15909=CARTESIAN_POINT('Ctrl Pts',(-12.9999999999738,13.000000000003,18.49999999892));
#15910=CARTESIAN_POINT('Ctrl Pts',(-13.6213203832862,10.9999999999767,20.5));
#15911=CARTESIAN_POINT('Ctrl Pts',(-13.6213203832735,13.0000000010845,20.5000000000236));
#15912=CARTESIAN_POINT('Ctrl Pts',(-13.6213203832599,13.0000000000145,18.4999999989158));
#15913=CARTESIAN_POINT('Ctrl Pts',(-14.0606602197355,10.9999999999847,20.0606601238272));
#15914=CARTESIAN_POINT('Ctrl Pts',(-14.0606602197256,12.5606601246825,20.0606601238456));
#15915=CARTESIAN_POINT('Ctrl Pts',(-14.0606602197151,12.5606601238475,18.4999999991479));
#15916=CARTESIAN_POINT('Ctrl Pts',(-14.5000000561849,10.9999999999927,19.6213202476545));
#15917=CARTESIAN_POINT('Ctrl Pts',(-14.5000000561778,12.1213202482804,19.6213202476677));
#15918=CARTESIAN_POINT('Ctrl Pts',(-14.5000000561702,12.1213202476805,18.4999999993799));
#15919=CARTESIAN_POINT('Ctrl Pts',(-14.5000000000041,11.,18.9999998643683));
#15920=CARTESIAN_POINT('Ctrl Pts',(-14.500000000001,11.4999998646618,18.9999998643742));
#15921=CARTESIAN_POINT('Ctrl Pts',(-14.4999999999976,11.4999998643943,18.4999999997124));
#15922=CARTESIAN_POINT('',(-14.4999999999976,11.5000000000041,18.4999999998461));
#15923=CARTESIAN_POINT('Origin',(-14.5000000000007,11.0000000000059,18.4999999999799));
#15924=CARTESIAN_POINT('Origin',(-13.0000000000016,11.500000000007,18.4999999997225));
#15925=CARTESIAN_POINT('Origin',(14.5,-42.5,-20.5));
#15926=CARTESIAN_POINT('',(14.5000000000008,-41.5,18.4999999994855));
#15927=CARTESIAN_POINT('',(14.5,-41.5,17.));
#15928=CARTESIAN_POINT('',(14.5,-41.5,-20.5));
#15929=CARTESIAN_POINT('',(14.5,11.5,17.));
#15930=CARTESIAN_POINT('',(14.5,-42.5,17.));
#15931=CARTESIAN_POINT('',(14.5,11.5,-20.5));
#15932=CARTESIAN_POINT('Ctrl Pts',(14.5000000000019,-41.5,18.4999999994855));
#15933=CARTESIAN_POINT('Ctrl Pts',(14.5000000000027,-41.5000000003692,18.7411872045814));
#15934=CARTESIAN_POINT('Ctrl Pts',(14.5000000000008,-41.241175036448,18.9975772517615));
#15935=CARTESIAN_POINT('Ctrl Pts',(14.5000000000013,-41.,18.9999999999984));
#15936=CARTESIAN_POINT('Origin',(13.,-41.,19.));
#15937=CARTESIAN_POINT('Ctrl Pts',(13.,-42.5,19.));
#15938=CARTESIAN_POINT('Ctrl Pts',(13.0022600019965,-42.5,19.0595135681432));
#15939=CARTESIAN_POINT('Ctrl Pts',(13.0073620228215,-42.4964573811086,19.1183481172834));
#15940=CARTESIAN_POINT('Ctrl Pts',(13.0153053530606,-42.4895493826963,19.1760919722096));
#15941=CARTESIAN_POINT('Ctrl Pts',(13.0166707573604,-42.4883619448773,19.186017747096));
#15942=CARTESIAN_POINT('Ctrl Pts',(13.0181201082026,-42.4870749459193,19.1959113155762));
#15943=CARTESIAN_POINT('Ctrl Pts',(13.0196533909879,-42.4856891362025,19.2057705877734));
#15944=CARTESIAN_POINT('Ctrl Pts',(13.0232674597544,-42.4824226731195,19.2290096719467));
#15945=CARTESIAN_POINT('Ctrl Pts',(13.0272781780523,-42.4786470144108,19.2518093521003));
#15946=CARTESIAN_POINT('Ctrl Pts',(13.0317575007208,-42.4743454279988,19.2744030249233));
#15947=CARTESIAN_POINT('Ctrl Pts',(13.0362018078404,-42.4700774677444,19.2968200795573));
#15948=CARTESIAN_POINT('Ctrl Pts',(13.0411074346211,-42.4652916250984,19.319034767169));
#15949=CARTESIAN_POINT('Ctrl Pts',(13.0465443279543,-42.4599219905355,19.3412644239973));
#15950=CARTESIAN_POINT('Ctrl Pts',(13.0514771601157,-42.4550501814998,19.3614331415751));
#15951=CARTESIAN_POINT('Ctrl Pts',(13.0568473243571,-42.4496972429146,19.381614336539));
#15952=CARTESIAN_POINT('Ctrl Pts',(13.0627066489669,-42.4437789851613,19.4019578562263));
#15953=CARTESIAN_POINT('Ctrl Pts',(13.0781595750634,-42.4281706333847,19.4556102696368));
#15954=CARTESIAN_POINT('Ctrl Pts',(13.096287694905,-42.4096294661813,19.5068516934207));
#15955=CARTESIAN_POINT('Ctrl Pts',(13.1170615404762,-42.3885021085325,19.5553003604737));
#15956=CARTESIAN_POINT('Ctrl Pts',(13.121596504369,-42.3838899723846,19.5658767823976));
#15957=CARTESIAN_POINT('Ctrl Pts',(13.1262574478728,-42.3791544387863,19.576320041403));
#15958=CARTESIAN_POINT('Ctrl Pts',(13.1310438701017,-42.3742988849167,19.5866260129124));
#15959=CARTESIAN_POINT('Ctrl Pts',(13.1443999464751,-42.3607499029811,19.61538389009));
#15960=CARTESIAN_POINT('Ctrl Pts',(13.1587334900202,-42.3462665987258,19.6430731920815));
#15961=CARTESIAN_POINT('Ctrl Pts',(13.1740297517328,-42.3309201189407,19.6696008381944));
#15962=CARTESIAN_POINT('Ctrl Pts',(13.1816778825891,-42.3232468790482,19.6828646612509));
#15963=CARTESIAN_POINT('Ctrl Pts',(13.1895666820893,-42.3153577656199,19.6958380292812));
#15964=CARTESIAN_POINT('Ctrl Pts',(13.1976935757618,-42.3072615166738,19.7085086994005));
#15965=CARTESIAN_POINT('Ctrl Pts',(13.201757022598,-42.3032133922008,19.7148440344601));
#15966=CARTESIAN_POINT('Ctrl Pts',(13.2058799925008,-42.2991134795606,19.7211036930466));
#15967=CARTESIAN_POINT('Ctrl Pts',(13.2100621289868,-42.2949628612153,19.7272861129147));
#15968=CARTESIAN_POINT('Ctrl Pts',(13.2129317585393,-42.2921148582616,19.7315282639825));
#15969=CARTESIAN_POINT('Ctrl Pts',(13.2161072666261,-42.2889722558305,19.7361264257699));
#15970=CARTESIAN_POINT('Ctrl Pts',(13.2190161563155,-42.2860911505925,19.7402712176225));
#15971=CARTESIAN_POINT('Ctrl Pts',(13.2203466199925,-42.284773394927,19.7421669564086));
#15972=CARTESIAN_POINT('Ctrl Pts',(13.2216213369746,-42.2835109849067,19.7439683311336));
#15973=CARTESIAN_POINT('Ctrl Pts',(13.2227856645689,-42.2823599620334,19.7456000774117));
#15974=CARTESIAN_POINT('Ctrl Pts',(13.2405637499002,-42.2647850261129,19.7705151654961));
#15975=CARTESIAN_POINT('Ctrl Pts',(13.2598640476569,-42.2459665645706,19.794609810812));
#15976=CARTESIAN_POINT('Ctrl Pts',(13.280640545793,-42.2258491150598,19.817639793041));
#15977=CARTESIAN_POINT('Ctrl Pts',(13.3008006762611,-42.2063284814975,19.8399865544333));
#15978=CARTESIAN_POINT('Ctrl Pts',(13.3223509770152,-42.1855841698294,19.8613306716809));
#15979=CARTESIAN_POINT('Ctrl Pts',(13.3452294106433,-42.1635863623897,19.8814099110445));
#15980=CARTESIAN_POINT('Ctrl Pts',(13.3680574656428,-42.1416369944276,19.9014449356443));
#15981=CARTESIAN_POINT('Ctrl Pts',(13.3922081789123,-42.118438919148,19.920220446142));
#15982=CARTESIAN_POINT('Ctrl Pts',(13.4175949294985,-42.0939937051849,19.9374391968938));
#15983=CARTESIAN_POINT('Ctrl Pts',(13.4413843219079,-42.0710866070304,19.9535745276856));
#15984=CARTESIAN_POINT('Ctrl Pts',(13.4662591457969,-42.0470841490337,19.9683422449708));
#15985=CARTESIAN_POINT('Ctrl Pts',(13.4921236617146,-42.0220212156595,19.9814718214613));
#15986=CARTESIAN_POINT('Ctrl Pts',(13.5174413758943,-41.9974881377666,19.9943238255717));
#15987=CARTESIAN_POINT('Ctrl Pts',(13.5437075604478,-41.9719385906071,20.0056057520624));
#15988=CARTESIAN_POINT('Ctrl Pts',(13.570806305913,-41.9454430912019,20.0150455765278));
#15989=CARTESIAN_POINT('Ctrl Pts',(13.5971431853015,-41.9196924979476,20.0242200056066));
#15990=CARTESIAN_POINT('Ctrl Pts',(13.6242665788035,-41.8930481880007,20.0316539195686));
#15991=CARTESIAN_POINT('Ctrl Pts',(13.6520430849402,-41.8656150102203,20.0370874936393));
#15992=CARTESIAN_POINT('Ctrl Pts',(13.6599625404344,-41.8577934422582,20.0386366786886));
#15993=CARTESIAN_POINT('Ctrl Pts',(13.6679349096588,-41.8499080132866,20.0400232205286));
#15994=CARTESIAN_POINT('Ctrl Pts',(13.6759566644666,-41.8419618070235,20.0412410399504));
#15995=CARTESIAN_POINT('Ctrl Pts',(13.6895615020067,-41.8284850992632,20.0433064527912));
#15996=CARTESIAN_POINT('Ctrl Pts',(13.7033084869149,-41.8148334295775,20.0448865414525));
#15997=CARTESIAN_POINT('Ctrl Pts',(13.717179038175,-41.8010238866563,20.0459517007053));
#15998=CARTESIAN_POINT('Ctrl Pts',(13.724114313805,-41.7941191151957,20.0464842803318));
#15999=CARTESIAN_POINT('Ctrl Pts',(13.7310804857782,-41.7871748806342,20.0468881344742));
#16000=CARTESIAN_POINT('Ctrl Pts',(13.7380750284017,-41.7801936070758,20.0471595809273));
#16001=CARTESIAN_POINT('Ctrl Pts',(13.7415722997135,-41.7767029702966,20.0472953041538));
#16002=CARTESIAN_POINT('Ctrl Pts',(13.7450766640847,-41.7732030742176,20.0473979260408));
#16003=CARTESIAN_POINT('Ctrl Pts',(13.7485878000073,-41.7696942321775,20.0474669897581));
#16004=CARTESIAN_POINT('Ctrl Pts',(13.7512425761001,-41.7670411904934,20.0475192089571));
#16005=CARTESIAN_POINT('Ctrl Pts',(13.7543988140343,-41.7638864585117,20.0475555844872));
#16006=CARTESIAN_POINT('Ctrl Pts',(13.7569273746179,-41.7613564491054,20.0475673281273));
#16007=CARTESIAN_POINT('Ctrl Pts',(13.7577430206971,-41.7605403356747,20.0475711163117));
#16008=CARTESIAN_POINT('Ctrl Pts',(13.7584934884386,-41.7597892758663,20.0475727773388));
#16009=CARTESIAN_POINT('Ctrl Pts',(13.7591411982523,-41.759141187524,20.0475730516392));
#16010=CARTESIAN_POINT('Ctrl Pts',(13.7804931212882,-41.737776786194,20.0475820940233));
#16011=CARTESIAN_POINT('Ctrl Pts',(13.8026529827082,-41.7156086502557,20.0462820505169));
#16012=CARTESIAN_POINT('Ctrl Pts',(13.8254839294119,-41.6927124027106,20.0434202458328));
#16013=CARTESIAN_POINT('Ctrl Pts',(13.8481437807808,-41.6699877398652,20.0405798875405));
#16014=CARTESIAN_POINT('Ctrl Pts',(13.8714648760683,-41.6465453989694,20.0362005538643));
#16015=CARTESIAN_POINT('Ctrl Pts',(13.8952849873058,-41.6225025400937,20.0300268826986));
#16016=CARTESIAN_POINT('Ctrl Pts',(13.9191050985433,-41.5984596812179,20.0238532115329));
#16017=CARTESIAN_POINT('Ctrl Pts',(13.9434244185068,-41.5738158694174,20.0158845175339));
#16018=CARTESIAN_POINT('Ctrl Pts',(13.9680493372696,-41.5487382983821,20.0058661742501));
#16019=CARTESIAN_POINT('Ctrl Pts',(13.9774576724811,-41.5391570202929,20.0020385095668));
#16020=CARTESIAN_POINT('Ctrl Pts',(13.9871299310897,-41.5292932146631,19.9978150358827));
#16021=CARTESIAN_POINT('Ctrl Pts',(13.9967972146374,-41.5194120987705,19.9932806172185));
#16022=CARTESIAN_POINT('Ctrl Pts',(14.0064058022661,-41.5095909771022,19.9887737297496));
#16023=CARTESIAN_POINT('Ctrl Pts',(14.0160093076807,-41.4997530911245,19.9839596557493));
#16024=CARTESIAN_POINT('Ctrl Pts',(14.0253653096026,-41.4901498663702,19.9789683806747));
#16025=CARTESIAN_POINT('Ctrl Pts',(14.0312956956529,-41.4840627759018,19.9758046160323));
#16026=CARTESIAN_POINT('Ctrl Pts',(14.0371270970891,-41.4780697607539,19.9725706227384));
#16027=CARTESIAN_POINT('Ctrl Pts',(14.0428025582095,-41.4722321415579,19.9693088409126));
#16028=CARTESIAN_POINT('Ctrl Pts',(14.0701611976478,-41.444091816856,19.9535853761571));
#16029=CARTESIAN_POINT('Ctrl Pts',(14.0963327095341,-41.4170311408489,19.9358471136713));
#16030=CARTESIAN_POINT('Ctrl Pts',(14.1212830788706,-41.3911979198333,19.9163451557992));
#16031=CARTESIAN_POINT('Ctrl Pts',(14.1394468349858,-41.3723914516857,19.9021478186062));
#16032=CARTESIAN_POINT('Ctrl Pts',(14.1569636554055,-41.3542343823022,19.8870160430856));
#16033=CARTESIAN_POINT('Ctrl Pts',(14.1738240978003,-41.3367668935452,19.871048245986));
#16034=CARTESIAN_POINT('Ctrl Pts',(14.1938343650591,-41.3160361730703,19.8520973857407));
#16035=CARTESIAN_POINT('Ctrl Pts',(14.2129199741926,-41.2962772848737,19.831969157362));
#16036=CARTESIAN_POINT('Ctrl Pts',(14.2310705495173,-41.277533093463,19.8108271604627));
#16037=CARTESIAN_POINT('Ctrl Pts',(14.2401458371797,-41.2681609977577,19.800256162013));
#16038=CARTESIAN_POINT('Ctrl Pts',(14.2489874564841,-41.2590421748574,19.7894316869671));
#16039=CARTESIAN_POINT('Ctrl Pts',(14.2575946377126,-41.2501796687351,19.778373856542));
#16040=CARTESIAN_POINT('Ctrl Pts',(14.2618982283269,-41.2457484156739,19.7728449413295));
#16041=CARTESIAN_POINT('Ctrl Pts',(14.2663517713443,-41.241168563312,19.7669825101897));
#16042=CARTESIAN_POINT('Ctrl Pts',(14.2706384453587,-41.2367626882401,19.7611973270011));
#16043=CARTESIAN_POINT('Ctrl Pts',(14.2749251193732,-41.2323568131681,19.7554121438125));
#16044=CARTESIAN_POINT('Ctrl Pts',(14.2790451446467,-41.2281247953352,19.7497046604192));
#16045=CARTESIAN_POINT('Ctrl Pts',(14.2827124379415,-41.224362680723,19.7445201065444));
#16046=CARTESIAN_POINT('Ctrl Pts',(14.2975068311355,-41.2091857645782,19.72360486405));
#16047=CARTESIAN_POINT('Ctrl Pts',(14.3123312731019,-41.1941459053188,19.7008120823962));
#16048=CARTESIAN_POINT('Ctrl Pts',(14.3269411120902,-41.1794304559121,19.6760414162875));
#16049=CARTESIAN_POINT('Ctrl Pts',(14.3413036351894,-41.1649641101715,19.6516900689212));
#16050=CARTESIAN_POINT('Ctrl Pts',(14.3554586875558,-41.1508114166492,19.6254266233223));
#16051=CARTESIAN_POINT('Ctrl Pts',(14.3691431631322,-41.1371752343504,19.5971850248702));
#16052=CARTESIAN_POINT('Ctrl Pts',(14.3779641249747,-41.1283854021742,19.5789805959956));
#16053=CARTESIAN_POINT('Ctrl Pts',(14.3865034944592,-41.1198922786354,19.5601396066395));
#16054=CARTESIAN_POINT('Ctrl Pts',(14.3947786423472,-41.1116665454347,19.5404841547009));
#16055=CARTESIAN_POINT('Ctrl Pts',(14.4028733946198,-41.1036201306248,19.5212571854187));
#16056=CARTESIAN_POINT('Ctrl Pts',(14.410715528531,-41.0958293476444,19.5012505187318));
#16057=CARTESIAN_POINT('Ctrl Pts',(14.4182846891418,-41.0882967432289,19.4802834847057));
#16058=CARTESIAN_POINT('Ctrl Pts',(14.4255810842607,-41.0810355869507,19.4600720276376));
#16059=CARTESIAN_POINT('Ctrl Pts',(14.4326239707515,-41.0740141774503,19.4389677887742));
#16060=CARTESIAN_POINT('Ctrl Pts',(14.4393582777847,-41.0672656586373,19.4168010068855));
#16061=CARTESIAN_POINT('Ctrl Pts',(14.4408457695643,-41.0657750277217,19.411904748714));
#16062=CARTESIAN_POINT('Ctrl Pts',(14.4423180536051,-41.0642978397888,19.4069566312962));
#16063=CARTESIAN_POINT('Ctrl Pts',(14.4437742694652,-41.0628346783189,19.4019548009798));
#16064=CARTESIAN_POINT('Ctrl Pts',(14.4516573514502,-41.0549139969553,19.3748778822768));
#16065=CARTESIAN_POINT('Ctrl Pts',(14.4582965000516,-41.0480624381763,19.3489100621108));
#16066=CARTESIAN_POINT('Ctrl Pts',(14.4639363713605,-41.042118421645,19.324216500453));
#16067=CARTESIAN_POINT('Ctrl Pts',(14.4661232995477,-41.039813557476,19.314641273808));
#16068=CARTESIAN_POINT('Ctrl Pts',(14.4681597602495,-41.0376451182981,19.3052571196166));
#16069=CARTESIAN_POINT('Ctrl Pts',(14.4700591414188,-41.0356036616017,19.2960717818563));
#16070=CARTESIAN_POINT('Ctrl Pts',(14.4734579900107,-41.0319505758862,19.2796350745664));
#16071=CARTESIAN_POINT('Ctrl Pts',(14.476418228949,-41.0287040152659,19.2638355064284));
#16072=CARTESIAN_POINT('Ctrl Pts',(14.4790122221541,-41.0258106568904,19.2487099851427));
#16073=CARTESIAN_POINT('Ctrl Pts',(14.4803092187566,-41.0243639777027,19.2411472244999));
#16074=CARTESIAN_POINT('Ctrl Pts',(14.481514544451,-41.0230055973116,19.2337529579336));
#16075=CARTESIAN_POINT('Ctrl Pts',(14.4826367188961,-41.0217290413751,19.2265308114627));
#16076=CARTESIAN_POINT('Ctrl Pts',(14.4833342254105,-41.0209355764324,19.2220417641192));
#16077=CARTESIAN_POINT('Ctrl Pts',(14.4839235680074,-41.0202614215225,19.2181274901393));
#16078=CARTESIAN_POINT('Ctrl Pts',(14.4845504272508,-41.0195394890262,19.2138416173666));
#16079=CARTESIAN_POINT('Ctrl Pts',(14.484932082493,-41.0190999496486,19.2112322184811));
#16080=CARTESIAN_POINT('Ctrl Pts',(14.4853270789767,-41.0186432748577,19.2084849018578));
#16081=CARTESIAN_POINT('Ctrl Pts',(14.4857618520254,-41.0181384289453,19.2053843140591));
#16082=CARTESIAN_POINT('Ctrl Pts',(14.4877126267577,-41.0158732456439,19.1914723469945));
#16083=CARTESIAN_POINT('Ctrl Pts',(14.489515707467,-41.0137373207059,19.1771172760478));
#16084=CARTESIAN_POINT('Ctrl Pts',(14.4911115466222,-41.0118111922518,19.1626248789929));
#16085=CARTESIAN_POINT('Ctrl Pts',(14.4926914198304,-41.0099043342014,19.1482774745222));
#16086=CARTESIAN_POINT('Ctrl Pts',(14.4940681434128,-41.0082032646087,19.1337957756093));
#16087=CARTESIAN_POINT('Ctrl Pts',(14.4952182617322,-41.0067485658386,19.1194855917744));
#16088=CARTESIAN_POINT('Ctrl Pts',(14.4956431563988,-41.0062111483064,19.1141989002344));
#16089=CARTESIAN_POINT('Ctrl Pts',(14.496037463468,-41.0057069741921,19.1089356844527));
#16090=CARTESIAN_POINT('Ctrl Pts',(14.4964011799049,-41.0052367471062,19.1037115483395));
#16091=CARTESIAN_POINT('Ctrl Pts',(14.4971421260223,-41.004278822475,19.0930691825373));
#16092=CARTESIAN_POINT('Ctrl Pts',(14.4977897638712,-41.0034179669619,19.082068267));
#16093=CARTESIAN_POINT('Ctrl Pts',(14.4983114829805,-41.0026999974748,19.0711014063315));
#16094=CARTESIAN_POINT('Ctrl Pts',(14.4986145428171,-41.0022829383494,19.0647308997844));
#16095=CARTESIAN_POINT('Ctrl Pts',(14.4988757478153,-41.0019133711413,19.0583720003773));
#16096=CARTESIAN_POINT('Ctrl Pts',(14.4990939964136,-41.0015941473328,19.052102289881));
#16097=CARTESIAN_POINT('Ctrl Pts',(14.4993692046759,-41.0011916108204,19.0441962774544));
#16098=CARTESIAN_POINT('Ctrl Pts',(14.4995892916705,-41.0008491769556,19.0359872297785));
#16099=CARTESIAN_POINT('Ctrl Pts',(14.4997384818162,-41.0005921979,19.0280024188491));
#16100=CARTESIAN_POINT('Ctrl Pts',(14.4997502855326,-41.0005718660751,19.0273706717324));
#16101=CARTESIAN_POINT('Ctrl Pts',(14.4997616629826,-41.0005520485121,19.0267403293932));
#16102=CARTESIAN_POINT('Ctrl Pts',(14.4997726153436,-41.0005327471464,19.0261116534472));
#16103=CARTESIAN_POINT('Ctrl Pts',(14.4998099608464,-41.000466933099,19.0239679860534));
#16104=CARTESIAN_POINT('Ctrl Pts',(14.4998429629253,-41.0004060665387,19.0218093930498));
#16105=CARTESIAN_POINT('Ctrl Pts',(14.4998714306183,-41.0003504001876,19.0196359067679));
#16106=CARTESIAN_POINT('Ctrl Pts',(14.4998913569851,-41.0003114357332,19.0181145441214));
#16107=CARTESIAN_POINT('Ctrl Pts',(14.4998972483194,-41.0002995822785,19.0176308540144));
#16108=CARTESIAN_POINT('Ctrl Pts',(14.4999147420325,-41.0002622818382,19.0159905547722));
#16109=CARTESIAN_POINT('Ctrl Pts',(14.4999222406152,-41.000246293212,19.0152874496266));
#16110=CARTESIAN_POINT('Ctrl Pts',(14.4999316961465,-41.0002258364841,19.0143718261369));
#16111=CARTESIAN_POINT('Ctrl Pts',(14.499943037045,-41.0001992580938,19.0130708039746));
#16112=CARTESIAN_POINT('Ctrl Pts',(14.4999813878673,-41.0001093795772,19.0086712169236));
#16113=CARTESIAN_POINT('Ctrl Pts',(14.4999919153304,-41.0000539915017,19.0053844424774));
#16114=CARTESIAN_POINT('Ctrl Pts',(14.4999965710787,-41.0000280644151,19.003207173894));
#16115=CARTESIAN_POINT('Ctrl Pts',(14.5000010927214,-41.0000028841408,19.0010926200623));
#16116=CARTESIAN_POINT('Ctrl Pts',(14.5,-41.0000001237228,19.0000246345942));
#16117=CARTESIAN_POINT('Ctrl Pts',(14.5,-41.,19.));
#16118=CARTESIAN_POINT('Origin',(-14.5,-42.5,-20.5));
#16119=CARTESIAN_POINT('',(13.5,-42.5,17.));
#16120=CARTESIAN_POINT('',(13.4999999999999,-42.4999999999994,18.4999999994848));
#16121=CARTESIAN_POINT('',(13.5,-42.5,-20.5));
#16122=CARTESIAN_POINT('Ctrl Pts',(13.4999999999999,-42.4999999999986,18.4999999994848));
#16123=CARTESIAN_POINT('Ctrl Pts',(13.5000000000266,-42.4999999999987,18.5175482730347));
#16124=CARTESIAN_POINT('Ctrl Pts',(13.4986337558358,-42.5000000000026,18.5351573548439));
#16125=CARTESIAN_POINT('Ctrl Pts',(13.4959747613953,-42.4999999999946,18.5528292058201));
#16126=CARTESIAN_POINT('Ctrl Pts',(13.4941761705346,-42.4999999999891,18.5647827583261));
#16127=CARTESIAN_POINT('Ctrl Pts',(13.4917848454981,-42.4999999999802,18.5767650851484));
#16128=CARTESIAN_POINT('Ctrl Pts',(13.4888102900511,-42.499999999916,18.5887750039491));
#16129=CARTESIAN_POINT('Ctrl Pts',(13.4863781587337,-42.4999999998636,18.5985948577578));
#16130=CARTESIAN_POINT('Ctrl Pts',(13.4834985579312,-42.4999999998589,18.6086211899905));
#16131=CARTESIAN_POINT('Ctrl Pts',(13.4802054497616,-42.4999999998767,18.6186663958456));
#16132=CARTESIAN_POINT('Ctrl Pts',(13.4768015227683,-42.4999999998951,18.6290496403681));
#16133=CARTESIAN_POINT('Ctrl Pts',(13.4729558419144,-42.4999999999242,18.6394525253292));
#16134=CARTESIAN_POINT('Ctrl Pts',(13.4687628721224,-42.4999999999245,18.6496758796856));
#16135=CARTESIAN_POINT('Ctrl Pts',(13.4647167019552,-42.4999999999248,18.6595413052567));
#16136=CARTESIAN_POINT('Ctrl Pts',(13.4603480054249,-42.4999999999231,18.6692392546691));
#16137=CARTESIAN_POINT('Ctrl Pts',(13.4557857876007,-42.499999999774,18.6786040936032));
#16138=CARTESIAN_POINT('Ctrl Pts',(13.4451257644337,-42.4999999994256,18.7004858633564));
#16139=CARTESIAN_POINT('Ctrl Pts',(13.4327339021801,-42.4999999992441,18.7218831631332));
#16140=CARTESIAN_POINT('Ctrl Pts',(13.4187879601852,-42.4999999993707,18.7426611284788));
#16141=CARTESIAN_POINT('Ctrl Pts',(13.4045377764472,-42.4999999995,18.7638923815546));
#16142=CARTESIAN_POINT('Ctrl Pts',(13.3886636880513,-42.499999999749,18.7844784249754));
#16143=CARTESIAN_POINT('Ctrl Pts',(13.3713104340802,-42.4999999997995,18.8042484071092));
#16144=CARTESIAN_POINT('Ctrl Pts',(13.3614729450939,-42.499999999828,18.8154559294462));
#16145=CARTESIAN_POINT('Ctrl Pts',(13.3511593888156,-42.4999999998311,18.8264005904639));
#16146=CARTESIAN_POINT('Ctrl Pts',(13.3403924032599,-42.4999999996694,18.8370447253153));
#16147=CARTESIAN_POINT('Ctrl Pts',(13.3283055921268,-42.4999999994878,18.848993626608));
#16148=CARTESIAN_POINT('Ctrl Pts',(13.3159610585321,-42.4999999993708,18.8602430590866));
#16149=CARTESIAN_POINT('Ctrl Pts',(13.303331566112,-42.499999999374,18.8708954642608));
#16150=CARTESIAN_POINT('Ctrl Pts',(13.2909314512315,-42.4999999993771,18.8813543998633));
#16151=CARTESIAN_POINT('Ctrl Pts',(13.2782554811413,-42.499999999477,18.8912384137336));
#16152=CARTESIAN_POINT('Ctrl Pts',(13.2652378046748,-42.4999999995746,18.9006092703813));
#16153=CARTESIAN_POINT('Ctrl Pts',(13.2518589264016,-42.499999999675,18.9102401404316));
#16154=CARTESIAN_POINT('Ctrl Pts',(13.2381182986558,-42.4999999997664,18.9193301169329));
#16155=CARTESIAN_POINT('Ctrl Pts',(13.2239161523732,-42.4999999997977,18.9278952079878));
#16156=CARTESIAN_POINT('Ctrl Pts',(13.2110597721419,-42.4999999998261,18.935648688703));
#16157=CARTESIAN_POINT('Ctrl Pts',(13.1978243246456,-42.4999999998288,18.9429720735206));
#16158=CARTESIAN_POINT('Ctrl Pts',(13.1841254335216,-42.4999999996881,18.9498297778044));
#16159=CARTESIAN_POINT('Ctrl Pts',(13.1826914760402,-42.4999999996733,18.9505476210426));
#16160=CARTESIAN_POINT('Ctrl Pts',(13.1812524367053,-42.4999999996567,18.9512603143427));
#16161=CARTESIAN_POINT('Ctrl Pts',(13.1798082169117,-42.4999999996377,18.9519677825118));
#16162=CARTESIAN_POINT('Ctrl Pts',(13.1618474281236,-42.499999999402,18.9607660876009));
#16163=CARTESIAN_POINT('Ctrl Pts',(13.1439125685113,-42.4999999992861,18.9683362971943));
#16164=CARTESIAN_POINT('Ctrl Pts',(13.1260291942023,-42.4999999993601,18.9747217350995));
#16165=CARTESIAN_POINT('Ctrl Pts',(13.1083133090592,-42.4999999994334,18.9810473693206));
#16166=CARTESIAN_POINT('Ctrl Pts',(13.0906467851646,-42.4999999996451,18.9862110000933));
#16167=CARTESIAN_POINT('Ctrl Pts',(13.0730280313959,-42.4999999997876,18.990211796952));
#16168=CARTESIAN_POINT('Ctrl Pts',(13.0561751561859,-42.4999999999239,18.9940386811394));
#16169=CARTESIAN_POINT('Ctrl Pts',(13.0393650740392,-42.4999999999852,18.9968019370571));
#16170=CARTESIAN_POINT('Ctrl Pts',(13.0225870886961,-42.4999999999965,18.9984547549262));
#16171=CARTESIAN_POINT('Ctrl Pts',(13.0150519404101,-42.5000000000015,18.9991970507072));
#16172=CARTESIAN_POINT('Ctrl Pts',(13.0075232175578,-42.5000000000005,18.9997147100955));
#16173=CARTESIAN_POINT('Ctrl Pts',(13.,-42.5000000000005,19.));
#16174=CARTESIAN_POINT('',(-13.5,-42.5000000000008,18.4999999994861));
#16175=CARTESIAN_POINT('Ctrl Pts',(-13.5,-42.5000000000019,18.4999999994861));
#16176=CARTESIAN_POINT('Ctrl Pts',(-13.5000000003688,-42.5000000000027,
18.7411872045822));
#16177=CARTESIAN_POINT('Ctrl Pts',(-13.2411750364478,-42.5000000000008,
18.9975772517629));
#16178=CARTESIAN_POINT('Ctrl Pts',(-13.,-42.5000000000013,18.9999999999985));
#16179=CARTESIAN_POINT('',(-13.5,-42.5,17.));
#16180=CARTESIAN_POINT('',(-13.5,-42.5,-20.5));
#16181=CARTESIAN_POINT('',(-14.5,-42.5,17.));
#16182=CARTESIAN_POINT('Origin',(-13.,-41.,19.));
#16183=CARTESIAN_POINT('Ctrl Pts',(-14.5000000000002,-41.,18.9999999095867));
#16184=CARTESIAN_POINT('Ctrl Pts',(-14.5,-41.0002683704709,19.0070720742973));
#16185=CARTESIAN_POINT('Ctrl Pts',(-14.5008952119788,-41.0008162323375,
19.0450824562715));
#16186=CARTESIAN_POINT('Ctrl Pts',(-14.4931017851684,-41.0110134479768,
19.1473283609849));
#16187=CARTESIAN_POINT('Ctrl Pts',(-14.4888014238237,-41.0161476273397,
19.1889301853449));
#16188=CARTESIAN_POINT('Ctrl Pts',(-14.4769322259473,-41.0289667632409,
19.2616359812436));
#16189=CARTESIAN_POINT('Ctrl Pts',(-14.4720622413127,-41.0341016700835,
19.2875788666429));
#16190=CARTESIAN_POINT('Ctrl Pts',(-14.4629416839819,-41.0434746813108,
19.3288153342504));
#16191=CARTESIAN_POINT('Ctrl Pts',(-14.457926662538,-41.0485793737959,19.3500126255628));
#16192=CARTESIAN_POINT('Ctrl Pts',(-14.4511743173683,-41.0553534003836,
19.3756863417945));
#16193=CARTESIAN_POINT('Ctrl Pts',(-14.4480754803318,-41.0584413889369,
19.3868828151956));
#16194=CARTESIAN_POINT('Ctrl Pts',(-14.4459627179151,-41.0605421677126,
19.3943891095111));
#16195=CARTESIAN_POINT('Ctrl Pts',(-14.4444040881135,-41.0620877097344,
19.3998091262352));
#16196=CARTESIAN_POINT('Ctrl Pts',(-14.4237756906892,-41.082512704408,19.470717215942));
#16197=CARTESIAN_POINT('Ctrl Pts',(-14.3993690637951,-41.1063530632061,
19.5340649357977));
#16198=CARTESIAN_POINT('Ctrl Pts',(-14.3583270196759,-41.1468285268692,
19.6201464487667));
#16199=CARTESIAN_POINT('Ctrl Pts',(-14.3439056403296,-41.1611049530719,
19.6473572697789));
#16200=CARTESIAN_POINT('Ctrl Pts',(-14.3139153763818,-41.1909975274763,
19.6987524160638));
#16201=CARTESIAN_POINT('Ctrl Pts',(-14.2976357723493,-41.2073325510989,
19.7239445601018));
#16202=CARTESIAN_POINT('Ctrl Pts',(-14.2518083414019,-41.2536918915089,
19.788911112031));
#16203=CARTESIAN_POINT('Ctrl Pts',(-14.2168974150804,-41.2896437989156,
19.8306766770144));
#16204=CARTESIAN_POINT('Ctrl Pts',(-14.1571767183321,-41.3517717037646,
19.8879120782401));
#16205=CARTESIAN_POINT('Ctrl Pts',(-14.1360457868065,-41.373839332279,19.9060806952706));
#16206=CARTESIAN_POINT('Ctrl Pts',(-14.0912261827393,-41.4206695624726,
19.9400003402846));
#16207=CARTESIAN_POINT('Ctrl Pts',(-14.0688649668164,-41.4440503251661,
19.9549959653011));
#16208=CARTESIAN_POINT('Ctrl Pts',(-13.9898492874905,-41.5263333774401,
19.9999263838317));
#16209=CARTESIAN_POINT('Ctrl Pts',(-13.9384829545777,-41.5789080828669,
20.0192563633802));
#16210=CARTESIAN_POINT('Ctrl Pts',(-13.866731070959,-41.6514471380887,20.0371046073534));
#16211=CARTESIAN_POINT('Ctrl Pts',(-13.8436826949272,-41.6745978993848,
20.0411970669137));
#16212=CARTESIAN_POINT('Ctrl Pts',(-13.8107160108182,-41.707607683097,20.0451193489531));
#16213=CARTESIAN_POINT('Ctrl Pts',(-13.7946330526831,-41.7236851791086,
20.0465257906122));
#16214=CARTESIAN_POINT('Ctrl Pts',(-13.7766256908422,-41.7416724003402,
20.0473128143693));
#16215=CARTESIAN_POINT('Ctrl Pts',(-13.7690755742822,-41.7492147607254,
20.0474791032033));
#16216=CARTESIAN_POINT('Ctrl Pts',(-13.7640799210929,-41.754205865215,20.0475532708898));
#16217=CARTESIAN_POINT('Ctrl Pts',(-13.7625698364561,-41.7557145519479,
20.0475716004369));
#16218=CARTESIAN_POINT('Ctrl Pts',(-13.6494244217153,-41.8687938800138,
20.047619490084));
#16219=CARTESIAN_POINT('Ctrl Pts',(-13.5458171257079,-41.9707644713532,
20.014226165779));
#16220=CARTESIAN_POINT('Ctrl Pts',(-13.4098535901852,-42.1031060930784,
19.9326926928269));
#16221=CARTESIAN_POINT('Ctrl Pts',(-13.3676863827572,-42.1439053577592,
19.9002696352513));
#16222=CARTESIAN_POINT('Ctrl Pts',(-13.3098169226224,-42.1998618651295,
19.8458099780668));
#16223=CARTESIAN_POINT('Ctrl Pts',(-13.2914204068261,-42.2176450616891,
19.8266825482741));
#16224=CARTESIAN_POINT('Ctrl Pts',(-13.2652190679525,-42.2430175435658,
19.796751892831));
#16225=CARTESIAN_POINT('Ctrl Pts',(-13.2567173583245,-42.2512581854533,
19.7865681729868));
#16226=CARTESIAN_POINT('Ctrl Pts',(-13.240185134444,-42.2673080364076,19.7658209853051));
#16227=CARTESIAN_POINT('Ctrl Pts',(-13.2329761306684,-42.2743164823624,
19.7563895777004));
#16228=CARTESIAN_POINT('Ctrl Pts',(-13.1899088809412,-42.3162962602579,
19.6970422219206));
#16229=CARTESIAN_POINT('Ctrl Pts',(-13.1591326285696,-42.3469593113915,
19.644299869016));
#16230=CARTESIAN_POINT('Ctrl Pts',(-13.1187018339568,-42.387576618264,19.5583253785839));
#16231=CARTESIAN_POINT('Ctrl Pts',(-13.1061787094213,-42.4002185564297,
19.5285226500102));
#16232=CARTESIAN_POINT('Ctrl Pts',(-13.0830590577013,-42.4235267889694,
19.4667920197459));
#16233=CARTESIAN_POINT('Ctrl Pts',(-13.0729799647175,-42.4336781543728,
19.4366329174016));
#16234=CARTESIAN_POINT('Ctrl Pts',(-13.0222535327245,-42.4841587298348,
19.2632423352929));
#16235=CARTESIAN_POINT('Ctrl Pts',(-13.0012852487877,-42.5,19.1269410506494));
#16236=CARTESIAN_POINT('Ctrl Pts',(-13.,-42.5000000000004,18.9999999999985));
#16237=CARTESIAN_POINT('Origin',(-14.5,13.,-20.5));
#16238=CARTESIAN_POINT('',(-14.5,11.5,17.));
#16239=CARTESIAN_POINT('',(-14.5,11.5,-20.5));
#16240=CARTESIAN_POINT('',(-14.5,-41.5,17.));
#16241=CARTESIAN_POINT('',(-14.5,13.,17.));
#16242=CARTESIAN_POINT('',(-14.4999999999994,-41.4999999999999,18.4999999994854));
#16243=CARTESIAN_POINT('',(-14.5,-41.5,-20.5));
#16244=CARTESIAN_POINT('Ctrl Pts',(-14.4999999999986,-41.5,18.4999999994854));
#16245=CARTESIAN_POINT('Ctrl Pts',(-14.4999999999987,-41.5000000000266,
18.5175482730428));
#16246=CARTESIAN_POINT('Ctrl Pts',(-14.5000000000027,-41.4986337558346,
18.5351573548596));
#16247=CARTESIAN_POINT('Ctrl Pts',(-14.4999999999946,-41.4959747613919,
18.5528292058435));
#16248=CARTESIAN_POINT('Ctrl Pts',(-14.4999999999891,-41.4941761705316,
18.564782758342));
#16249=CARTESIAN_POINT('Ctrl Pts',(-14.4999999999802,-41.4917848454962,
18.5767650851567));
#16250=CARTESIAN_POINT('Ctrl Pts',(-14.499999999916,-41.4888102900512,18.5887750039498));
#16251=CARTESIAN_POINT('Ctrl Pts',(-14.4999999998636,-41.4863781587332,
18.5985948577608));
#16252=CARTESIAN_POINT('Ctrl Pts',(-14.4999999998589,-41.4834985579299,
18.6086211899957));
#16253=CARTESIAN_POINT('Ctrl Pts',(-14.4999999998767,-41.4802054497594,
18.618666395853));
#16254=CARTESIAN_POINT('Ctrl Pts',(-14.4999999998951,-41.4768015227651,
18.6290496403776));
#16255=CARTESIAN_POINT('Ctrl Pts',(-14.4999999999242,-41.4729558419101,
18.6394525253408));
#16256=CARTESIAN_POINT('Ctrl Pts',(-14.4999999999246,-41.4687628721168,
18.6496758796993));
#16257=CARTESIAN_POINT('Ctrl Pts',(-14.4999999999249,-41.4647167019513,
18.6595413052655));
#16258=CARTESIAN_POINT('Ctrl Pts',(-14.4999999999231,-41.4603480054228,
18.6692392546731));
#16259=CARTESIAN_POINT('Ctrl Pts',(-14.499999999774,-41.4557857876006,18.6786040936032));
#16260=CARTESIAN_POINT('Ctrl Pts',(-14.4999999994256,-41.445125764451,18.7004858633204));
#16261=CARTESIAN_POINT('Ctrl Pts',(-14.4999999992441,-41.4327339022211,
18.721883163062));
#16262=CARTESIAN_POINT('Ctrl Pts',(-14.4999999993707,-41.4187879602549,
18.7426611283747));
#16263=CARTESIAN_POINT('Ctrl Pts',(-14.4999999995,-41.4045377765463,18.7638923814168));
#16264=CARTESIAN_POINT('Ctrl Pts',(-14.499999999749,-41.388663688185,18.7844784248062));
#16265=CARTESIAN_POINT('Ctrl Pts',(-14.4999999997995,-41.3713104342529,
18.8042484069122));
#16266=CARTESIAN_POINT('Ctrl Pts',(-14.4999999998281,-41.3614729452147,
18.8154559293178));
#16267=CARTESIAN_POINT('Ctrl Pts',(-14.4999999998311,-41.3511593888788,
18.8264005904013));
#16268=CARTESIAN_POINT('Ctrl Pts',(-14.4999999996694,-41.3403924032599,
18.8370447253151));
#16269=CARTESIAN_POINT('Ctrl Pts',(-14.4999999994878,-41.3283055921264,
18.848993626608));
#16270=CARTESIAN_POINT('Ctrl Pts',(-14.4999999993708,-41.3159610585317,
18.8602430590867));
#16271=CARTESIAN_POINT('Ctrl Pts',(-14.499999999374,-41.3033315661115,18.8708954642609));
#16272=CARTESIAN_POINT('Ctrl Pts',(-14.4999999993771,-41.2909314512325,
18.8813543998622));
#16273=CARTESIAN_POINT('Ctrl Pts',(-14.499999999477,-41.2782554811439,18.8912384137313));
#16274=CARTESIAN_POINT('Ctrl Pts',(-14.4999999995746,-41.2652378046791,
18.900609270378));
#16275=CARTESIAN_POINT('Ctrl Pts',(-14.499999999675,-41.2518589264053,18.910240140429));
#16276=CARTESIAN_POINT('Ctrl Pts',(-14.4999999997664,-41.2381182986589,
18.9193301169308));
#16277=CARTESIAN_POINT('Ctrl Pts',(-14.4999999997977,-41.2239161523756,
18.9278952079862));
#16278=CARTESIAN_POINT('Ctrl Pts',(-14.4999999998261,-41.211059772146,18.9356486887005));
#16279=CARTESIAN_POINT('Ctrl Pts',(-14.4999999998288,-41.1978243246514,
18.9429720735174));
#16280=CARTESIAN_POINT('Ctrl Pts',(-14.4999999996881,-41.1841254335292,
18.9498297778006));
#16281=CARTESIAN_POINT('Ctrl Pts',(-14.4999999996733,-41.1826914760453,
18.95054762104));
#16282=CARTESIAN_POINT('Ctrl Pts',(-14.4999999996567,-41.1812524367078,
18.9512603143414));
#16283=CARTESIAN_POINT('Ctrl Pts',(-14.4999999996378,-41.1798082169117,
18.9519677825117));
#16284=CARTESIAN_POINT('Ctrl Pts',(-14.499999999402,-41.161847433483,18.9607660849755));
#16285=CARTESIAN_POINT('Ctrl Pts',(-14.4999999992861,-41.1439125794643,
18.9683362925574));
#16286=CARTESIAN_POINT('Ctrl Pts',(-14.4999999993601,-41.1260292108387,
18.9747217291591));
#16287=CARTESIAN_POINT('Ctrl Pts',(-14.4999999994335,-41.108313331451,18.9810473620443));
#16288=CARTESIAN_POINT('Ctrl Pts',(-14.4999999996451,-41.0906468133997,
18.9862109921918));
#16289=CARTESIAN_POINT('Ctrl Pts',(-14.4999999997876,-41.0730280654294,
18.9902117892228));
#16290=CARTESIAN_POINT('Ctrl Pts',(-14.4999999999239,-41.0561751957912,
18.9940386735692));
#16291=CARTESIAN_POINT('Ctrl Pts',(-14.4999999999852,-41.0393651191756,
18.9968019303783));
#16292=CARTESIAN_POINT('Ctrl Pts',(-14.4999999999965,-41.0225871392088,
18.9984547499492));
#16293=CARTESIAN_POINT('Ctrl Pts',(-14.5000000000015,-41.0150519763219,
18.9991970481707));
#16294=CARTESIAN_POINT('Ctrl Pts',(-14.5000000000006,-41.0075232388665,
18.9997147091494));
#16295=CARTESIAN_POINT('Ctrl Pts',(-14.5000000000005,-41.0000000066869,
18.9999999997464));
#16296=CARTESIAN_POINT('Origin',(-13.94140536675,11.,17.13971317669));
#16297=CARTESIAN_POINT('',(-15.5952583708893,12.1246200428121,14.5));
#16298=CARTESIAN_POINT('',(-15.5952583708895,12.1246200428123,17.));
#16299=CARTESIAN_POINT('',(-15.5952583708915,12.124620042811,17.13971317669));
#16300=CARTESIAN_POINT('Origin',(-13.94140536675,11.,17.));
#16301=CARTESIAN_POINT('Origin',(-13.94140536675,11.,14.5));
#16302=CARTESIAN_POINT('Origin',(-12.5,11.,20.63971317669));
#16303=CARTESIAN_POINT('',(-14.5,11.,-14.5));
#16304=CARTESIAN_POINT('',(-14.5,11.,14.5));
#16305=CARTESIAN_POINT('',(-14.5,11.,20.63971317669));
#16306=CARTESIAN_POINT('Origin',(-12.5,11.,14.5));
#16307=CARTESIAN_POINT('Origin',(-12.5,11.,-14.5));
#16308=CARTESIAN_POINT('Origin',(-13.94140536675,11.,-12.36535464022));
#16309=CARTESIAN_POINT('',(-15.5952583708895,12.1246200428123,-17.));
#16310=CARTESIAN_POINT('',(-15.5952583708896,12.1246200428122,-14.5));
#16311=CARTESIAN_POINT('',(-15.5952583708915,12.124620042811,-12.36535464022));
#16312=CARTESIAN_POINT('Origin',(-13.94140536675,11.,-14.5));
#16313=CARTESIAN_POINT('Origin',(-13.94140536675,11.,-17.));
#16314=CARTESIAN_POINT('Origin',(0.,0.,-17.));
#16315=CARTESIAN_POINT('',(20.1,-39.67662948547,-17.));
#16316=CARTESIAN_POINT('',(20.1,4.576629485471,-17.));
#16317=CARTESIAN_POINT('',(20.1,0.,-17.));
#16318=CARTESIAN_POINT('',(19.5807795062094,-41.3635595496909,-17.));
#16319=CARTESIAN_POINT('Origin',(17.1,-39.67662948547,-17.));
#16320=CARTESIAN_POINT('',(15.8928875563296,-46.786930064221,-17.));
#16321=CARTESIAN_POINT('',(15.89288755633,-46.78693006422,-17.));
#16322=CARTESIAN_POINT('',(13.41210805012,-48.1,-17.));
#16323=CARTESIAN_POINT('Origin',(13.41210805012,-45.1,-17.));
#16324=CARTESIAN_POINT('',(-13.41210805012,-48.1,-17.));
#16325=CARTESIAN_POINT('',(0.,-48.1,-17.));
#16326=CARTESIAN_POINT('',(-15.8928875563294,-46.7869300642209,-17.));
#16327=CARTESIAN_POINT('Origin',(-13.41210805012,-45.1,-17.));
#16328=CARTESIAN_POINT('',(-19.5807795062097,-41.3635595496911,-17.));
#16329=CARTESIAN_POINT('',(-19.58077950621,-41.36355954969,-17.));
#16330=CARTESIAN_POINT('',(-20.1,-39.67662948547,-17.));
#16331=CARTESIAN_POINT('Origin',(-17.1,-39.67662948547,-17.));
#16332=CARTESIAN_POINT('',(-20.1,4.576629485471,-17.));
#16333=CARTESIAN_POINT('',(-20.1,0.,-17.));
#16334=CARTESIAN_POINT('',(-19.5807795062095,6.26355954969313,-17.));
#16335=CARTESIAN_POINT('Origin',(-17.1,4.576629485471,-17.));
#16336=CARTESIAN_POINT('',(-15.59525837089,12.12462004281,-17.));
#16337=CARTESIAN_POINT('',(-8.15,11.5,-17.));
#16338=CARTESIAN_POINT('Origin',(-6.65,11.5,-17.));
#16339=CARTESIAN_POINT('',(-8.15,9.,-17.));
#16340=CARTESIAN_POINT('',(-8.15,0.,-17.));
#16341=CARTESIAN_POINT('',(-10.5,6.65,-17.));
#16342=CARTESIAN_POINT('Origin',(-10.5,9.,-17.));
#16343=CARTESIAN_POINT('',(-13.5,6.65,-17.));
#16344=CARTESIAN_POINT('',(0.,6.65,-17.));
#16345=CARTESIAN_POINT('',(-14.5,5.65,-17.));
#16346=CARTESIAN_POINT('Origin',(-13.5,5.65,-17.));
#16347=CARTESIAN_POINT('',(-14.5,-35.15,-17.));
#16348=CARTESIAN_POINT('',(-14.5,0.,-17.));
#16349=CARTESIAN_POINT('',(-13.5,-36.15,-17.));
#16350=CARTESIAN_POINT('Origin',(-13.5,-35.15,-17.));
#16351=CARTESIAN_POINT('',(-10.5,-36.15,-17.));
#16352=CARTESIAN_POINT('',(0.,-36.15,-17.));
#16353=CARTESIAN_POINT('',(-8.15,-38.5,-17.));
#16354=CARTESIAN_POINT('Origin',(-10.5,-38.5,-17.));
#16355=CARTESIAN_POINT('',(-8.15,-41.5,-17.));
#16356=CARTESIAN_POINT('',(-8.15,0.,-17.));
#16357=CARTESIAN_POINT('',(-7.15,-42.5,-17.));
#16358=CARTESIAN_POINT('Origin',(-7.15,-41.5,-17.));
#16359=CARTESIAN_POINT('',(7.15,-42.5,-17.));
#16360=CARTESIAN_POINT('',(0.,-42.5,-17.));
#16361=CARTESIAN_POINT('',(8.15,-41.5,-17.));
#16362=CARTESIAN_POINT('Origin',(7.15,-41.5,-17.));
#16363=CARTESIAN_POINT('',(8.15,-38.5,-17.));
#16364=CARTESIAN_POINT('',(8.15,0.,-17.));
#16365=CARTESIAN_POINT('',(10.5,-36.15,-17.));
#16366=CARTESIAN_POINT('Origin',(10.5,-38.5,-17.));
#16367=CARTESIAN_POINT('',(13.5,-36.15,-17.));
#16368=CARTESIAN_POINT('',(0.,-36.15,-17.));
#16369=CARTESIAN_POINT('',(14.5,-35.15,-17.));
#16370=CARTESIAN_POINT('Origin',(13.5,-35.15,-17.));
#16371=CARTESIAN_POINT('',(14.5,5.65,-17.));
#16372=CARTESIAN_POINT('',(14.5,0.,-17.));
#16373=CARTESIAN_POINT('',(13.5,6.65,-17.));
#16374=CARTESIAN_POINT('Origin',(13.5,5.65,-17.));
#16375=CARTESIAN_POINT('',(10.5,6.65,-17.));
#16376=CARTESIAN_POINT('',(0.,6.65,-17.));
#16377=CARTESIAN_POINT('',(8.15,9.000000000459,-17.));
#16378=CARTESIAN_POINT('Origin',(10.5,9.,-17.));
#16379=CARTESIAN_POINT('',(8.15,11.5,-17.));
#16380=CARTESIAN_POINT('',(8.15,0.,-17.));
#16381=CARTESIAN_POINT('Origin',(6.64999999999999,11.5,-17.));
#16382=CARTESIAN_POINT('',(15.5952583708895,12.1246200428123,-17.));
#16383=CARTESIAN_POINT('Origin',(13.94140536675,11.,-17.));
#16384=CARTESIAN_POINT('',(19.5807795062092,6.26355954969299,-17.));
#16385=CARTESIAN_POINT('',(19.58077950621,6.263559549693,-17.));
#16386=CARTESIAN_POINT('Origin',(17.1,4.576629485471,-17.));
#16387=CARTESIAN_POINT('Origin',(-14.64391314335,9.5,-17.));
#16388=CARTESIAN_POINT('',(-6.65,9.5,-20.5));
#16389=CARTESIAN_POINT('Origin',(-6.65,9.5,-17.));
#16390=CARTESIAN_POINT('',(6.650000000118,9.5,-20.5));
#16391=CARTESIAN_POINT('Origin',(6.65,9.5,-17.));
#16392=CARTESIAN_POINT('',(-14.64391314335,9.5,-20.5));
#16393=CARTESIAN_POINT('Origin',(13.94140536675,11.,-12.38062237617));
#16394=CARTESIAN_POINT('',(15.5952583708891,12.124620042812,-14.5));
#16395=CARTESIAN_POINT('Origin',(13.94140536675,11.,-14.5));
#16396=CARTESIAN_POINT('',(15.5952583708915,12.124620042811,-12.38062237617));
#16397=CARTESIAN_POINT('Origin',(12.5,11.,20.63971317669));
#16398=CARTESIAN_POINT('',(14.5,11.,14.5));
#16399=CARTESIAN_POINT('Origin',(12.5,11.,14.5));
#16400=CARTESIAN_POINT('',(14.5,11.,-14.5));
#16401=CARTESIAN_POINT('',(14.5,11.,20.63971317669));
#16402=CARTESIAN_POINT('Origin',(12.5,11.,-14.5));
#16403=CARTESIAN_POINT('Origin',(13.94140536675,11.,17.20607693562));
#16404=CARTESIAN_POINT('',(15.5952583708895,12.1246200428123,17.));
#16405=CARTESIAN_POINT('Origin',(13.94140536675,11.,17.));
#16406=CARTESIAN_POINT('',(15.5952583708896,12.1246200428122,14.5));
#16407=CARTESIAN_POINT('',(15.5952583708915,12.124620042811,17.20607693562));
#16408=CARTESIAN_POINT('Origin',(13.94140536675,11.,14.5));
#16409=CARTESIAN_POINT('Origin',(13.,11.5,18.63971317669));
#16410=CARTESIAN_POINT('Origin',(13.,11.5,17.));
#16411=CARTESIAN_POINT('Origin',(-13.,11.5,-17.13464535978));
#16412=CARTESIAN_POINT('Origin',(-13.,11.5,17.));
#16413=CARTESIAN_POINT('Origin',(0.,0.,17.));
#16414=CARTESIAN_POINT('',(19.5807795062093,-41.3635595496909,17.));
#16415=CARTESIAN_POINT('',(20.1,-39.67662948547,17.));
#16416=CARTESIAN_POINT('Origin',(17.1,-39.67662948547,17.));
#16417=CARTESIAN_POINT('',(20.1,4.576629485471,17.));
#16418=CARTESIAN_POINT('',(20.1,0.,17.));
#16419=CARTESIAN_POINT('',(19.5807795062093,6.26355954969304,17.));
#16420=CARTESIAN_POINT('Origin',(17.1,4.576629485471,17.));
#16421=CARTESIAN_POINT('',(19.58077950621,6.263559549693,17.));
#16422=CARTESIAN_POINT('Origin',(13.5,-41.5,17.));
#16423=CARTESIAN_POINT('Origin',(-13.5,-41.5,17.));
#16424=CARTESIAN_POINT('',(-19.5807795062095,6.26355954969313,17.));
#16425=CARTESIAN_POINT('',(-15.59525837089,12.12462004281,17.));
#16426=CARTESIAN_POINT('',(-20.1,4.576629485471,17.));
#16427=CARTESIAN_POINT('Origin',(-17.1,4.576629485471,17.));
#16428=CARTESIAN_POINT('',(-20.1,-39.67662948547,17.));
#16429=CARTESIAN_POINT('',(-20.1,0.,17.));
#16430=CARTESIAN_POINT('',(-19.5807795062097,-41.3635595496911,17.));
#16431=CARTESIAN_POINT('Origin',(-17.1,-39.67662948547,17.));
#16432=CARTESIAN_POINT('',(-15.8928875563294,-46.7869300642209,17.));
#16433=CARTESIAN_POINT('',(-19.58077950621,-41.36355954969,17.));
#16434=CARTESIAN_POINT('',(-13.41210805012,-48.1,17.));
#16435=CARTESIAN_POINT('Origin',(-13.41210805012,-45.1,17.));
#16436=CARTESIAN_POINT('',(13.41210805012,-48.1,17.));
#16437=CARTESIAN_POINT('',(0.,-48.1,17.));
#16438=CARTESIAN_POINT('',(15.8928875563296,-46.786930064221,17.));
#16439=CARTESIAN_POINT('Origin',(13.41210805012,-45.1,17.));
#16440=CARTESIAN_POINT('',(15.89288755633,-46.78693006422,17.));
#16441=CARTESIAN_POINT('Origin',(13.5,-41.5,20.63971317669));
#16442=CARTESIAN_POINT('Origin',(13.5,-41.5,18.4999999994851));
#16443=CARTESIAN_POINT('Ctrl Pts',(14.5000000000013,-40.9943380969227,19.0000100692442));
#16444=CARTESIAN_POINT('Ctrl Pts',(14.5000000000008,-41.2371059113903,19.0015933091084));
#16445=CARTESIAN_POINT('Ctrl Pts',(14.5000000000027,-41.5000000009281,18.7430757267126));
#16446=CARTESIAN_POINT('Ctrl Pts',(14.5000000000019,-41.5,18.4999999987137));
#16447=CARTESIAN_POINT('Ctrl Pts',(14.5000000000028,-40.995317328355,19.1412652085388));
#16448=CARTESIAN_POINT('Ctrl Pts',(14.5000000000014,-41.2564831044291,19.0954746833564));
#16449=CARTESIAN_POINT('Ctrl Pts',(14.5000000000026,-41.5369365607809,18.7901585471376));
#16450=CARTESIAN_POINT('Ctrl Pts',(14.5000000000014,-41.565449847102,18.4999999984638));
#16451=CARTESIAN_POINT('Ctrl Pts',(14.461088950263,-41.0396947394679,19.4141933256417));
#16452=CARTESIAN_POINT('Ctrl Pts',(14.4808879882492,-41.3232890737612,19.2739493035027));
#16453=CARTESIAN_POINT('Ctrl Pts',(14.4987197414757,-41.622688121818,18.8825190881865));
#16454=CARTESIAN_POINT('Ctrl Pts',(14.4871066327079,-41.6963473912737,18.4999999979725));
#16455=CARTESIAN_POINT('Ctrl Pts',(14.2951753510104,-41.2092320493177,19.7671081794723));
#16456=CARTESIAN_POINT('Ctrl Pts',(14.3829355447186,-41.4926490904922,19.5234352013656));
#16457=CARTESIAN_POINT('Ctrl Pts',(14.466126570005,-41.798927508403,18.9987393235418));
#16458=CARTESIAN_POINT('Ctrl Pts',(14.4298332811675,-41.8851496535818,18.4999999973609));
#16459=CARTESIAN_POINT('Ctrl Pts',(14.0470778370451,-41.4604801612305,20.0000694996508));
#16460=CARTESIAN_POINT('Ctrl Pts',(14.208692992919,-41.7204167792393,19.7008597170388));
#16461=CARTESIAN_POINT('Ctrl Pts',(14.373854422343,-42.0097950503571,19.0757337060923));
#16462=CARTESIAN_POINT('Ctrl Pts',(14.3368285937893,-42.059150964628,18.4999999969561));
#16463=CARTESIAN_POINT('Ctrl Pts',(13.7542691791144,-41.7542035734038,20.0822650788914));
#16464=CARTESIAN_POINT('Ctrl Pts',(13.9755845401677,-41.9754027621767,19.7657545358299));
#16465=CARTESIAN_POINT('Ctrl Pts',(14.2147126834794,-42.214781365487,19.1045289473882));
#16466=CARTESIAN_POINT('Ctrl Pts',(14.2116652821725,-42.2116652821764,18.4999999967981));
#16467=CARTESIAN_POINT('Ctrl Pts',(13.4602188374819,-42.0470674075824,20.0001437555219));
#16468=CARTESIAN_POINT('Ctrl Pts',(13.7204012871743,-42.209895391559,19.6998305081936));
#16469=CARTESIAN_POINT('Ctrl Pts',(14.0099355358227,-42.373720179787,19.0761517589292));
#16470=CARTESIAN_POINT('Ctrl Pts',(14.0591509646221,-42.3368285937868,18.4999999969514));
#16471=CARTESIAN_POINT('Ctrl Pts',(13.2100966184005,-42.2951361405335,19.7669964902518));
#16472=CARTESIAN_POINT('Ctrl Pts',(13.4934675131165,-42.3844114694822,19.5204897565771));
#16473=CARTESIAN_POINT('Ctrl Pts',(13.7991208871267,-42.4661360608768,18.9989428562529));
#16474=CARTESIAN_POINT('Ctrl Pts',(13.8851496535816,-42.4298332811645,18.4999999973594));
#16475=CARTESIAN_POINT('Ctrl Pts',(13.0371194604123,-42.4610525148315,19.4147999538865));
#16476=CARTESIAN_POINT('Ctrl Pts',(13.3212465098146,-42.4824926046905,19.2710925155892));
#16477=CARTESIAN_POINT('Ctrl Pts',(13.6219561650579,-42.4987406155644,18.8812429548123));
#16478=CARTESIAN_POINT('Ctrl Pts',(13.6963473912789,-42.4871066327043,18.4999999979835));
#16479=CARTESIAN_POINT('Ctrl Pts',(12.9992279345901,-42.5000000000002,19.1406085881773));
#16480=CARTESIAN_POINT('Ctrl Pts',(13.2589309435621,-42.5000000000008,19.0886851287514));
#16481=CARTESIAN_POINT('Ctrl Pts',(13.5382388686105,-42.4999999999992,18.7898907052044));
#16482=CARTESIAN_POINT('Ctrl Pts',(13.5654498470941,-42.4999999999989,18.4999999984642));
#16483=CARTESIAN_POINT('Ctrl Pts',(12.9943419397749,-42.5000000000005,19.0001703298077));
#16484=CARTESIAN_POINT('Ctrl Pts',(13.2369423184852,-42.5000000000009,18.9947709047232));
#16485=CARTESIAN_POINT('Ctrl Pts',(13.5000000009278,-42.4999999999995,18.7430757267406));
#16486=CARTESIAN_POINT('Ctrl Pts',(13.4999999999998,-42.4999999999986,18.499999998712));
#16487=CARTESIAN_POINT('Origin',(-13.5,-41.5,20.63971317669));
#16488=CARTESIAN_POINT('Origin',(-13.5,-41.5,18.4999999994858));
#16489=CARTESIAN_POINT('Ctrl Pts',(-12.9943339615788,-42.4999998766974,
18.9993941198875));
#16490=CARTESIAN_POINT('Ctrl Pts',(-13.2370215093323,-42.4999999394458,
19.001183925909));
#16491=CARTESIAN_POINT('Ctrl Pts',(-13.4998389829741,-42.4999999959596,
18.7428704243726));
#16492=CARTESIAN_POINT('Ctrl Pts',(-13.4997146170715,-42.4999999591457,
18.4999999987164));
#16493=CARTESIAN_POINT('Ctrl Pts',(-12.9952528645595,-42.5000565171419,
19.1408685031104));
#16494=CARTESIAN_POINT('Ctrl Pts',(-13.2563860300876,-42.500027753833,19.0952152741976));
#16495=CARTESIAN_POINT('Ctrl Pts',(-13.5368119425112,-42.5000018499864,
18.7900242984701));
#16496=CARTESIAN_POINT('Ctrl Pts',(-13.5652595922869,-42.500018726424,18.4999999984663));
#16497=CARTESIAN_POINT('Ctrl Pts',(-13.0396126018465,-42.4611693322662,
19.4140223450644));
#16498=CARTESIAN_POINT('Ctrl Pts',(-13.3232070220341,-42.4809354443569,
19.2738284322996));
#16499=CARTESIAN_POINT('Ctrl Pts',(-13.6226027371649,-42.4987355322512,
18.8824627816802));
#16500=CARTESIAN_POINT('Ctrl Pts',(-13.6962559201454,-42.4871343805644,
18.4999999979752));
#16501=CARTESIAN_POINT('Ctrl Pts',(-13.2092320493188,-42.2951753510108,
19.7671081794714));
#16502=CARTESIAN_POINT('Ctrl Pts',(-13.4926490904924,-42.3829355447187,
19.5234352013648));
#16503=CARTESIAN_POINT('Ctrl Pts',(-13.7989275084019,-42.4661265700046,
18.9987393235433));
#16504=CARTESIAN_POINT('Ctrl Pts',(-13.8851496535813,-42.4298332811677,
18.499999997364));
#16505=CARTESIAN_POINT('Ctrl Pts',(-13.4604801612315,-42.0470778370458,
20.0000694996497));
#16506=CARTESIAN_POINT('Ctrl Pts',(-13.7204167792395,-42.2086929929191,
19.7008597170379));
#16507=CARTESIAN_POINT('Ctrl Pts',(-14.009795050356,-42.3738544223422,19.0757337060942));
#16508=CARTESIAN_POINT('Ctrl Pts',(-14.0591509646277,-42.3368285937896,
18.4999999969598));
#16509=CARTESIAN_POINT('Ctrl Pts',(-13.7542035734047,-41.7542691791153,
20.0822650788902));
#16510=CARTESIAN_POINT('Ctrl Pts',(-13.9754027621768,-41.9755845401679,
19.7657545358289));
#16511=CARTESIAN_POINT('Ctrl Pts',(-14.214781365486,-42.2147126834784,19.1045289473902));
#16512=CARTESIAN_POINT('Ctrl Pts',(-14.2116652821764,-42.2116652821725,
18.4999999968019));
#16513=CARTESIAN_POINT('Ctrl Pts',(-14.047067407583,-41.4602188374757,20.0001437555207));
#16514=CARTESIAN_POINT('Ctrl Pts',(-14.209895391559,-41.7204012871736,19.6998305081927));
#16515=CARTESIAN_POINT('Ctrl Pts',(-14.3737201797862,-42.0099355358214,
19.0761517589311));
#16516=CARTESIAN_POINT('Ctrl Pts',(-14.336828593787,-42.0591509646218,18.499999996955));
#16517=CARTESIAN_POINT('Ctrl Pts',(-14.2951361405339,-41.2100966184016,
19.7669964902508));
#16518=CARTESIAN_POINT('Ctrl Pts',(-14.3844114694822,-41.4934675131167,
19.5204897565763));
#16519=CARTESIAN_POINT('Ctrl Pts',(-14.4661360608765,-41.7991208871255,
18.9989428562544));
#16520=CARTESIAN_POINT('Ctrl Pts',(-14.4298332811648,-41.8851496535811,
18.4999999973626));
#16521=CARTESIAN_POINT('Ctrl Pts',(-14.4611328981796,-41.0370356562491,
19.4146293213196));
#16522=CARTESIAN_POINT('Ctrl Pts',(-14.482540123147,-41.3211630719932,19.2709716873381));
#16523=CARTESIAN_POINT('Ctrl Pts',(-14.498756411855,-41.6218703320968,18.8811859314354));
#16524=CARTESIAN_POINT('Ctrl Pts',(-14.4871343805609,-41.6962559201502,
18.4999999979862));
#16525=CARTESIAN_POINT('Ctrl Pts',(-14.5000565701147,-40.9991729022973,
19.1402100457667));
#16526=CARTESIAN_POINT('Ctrl Pts',(-14.5000254207208,-41.2588403991452,
19.0884200014296));
#16527=CARTESIAN_POINT('Ctrl Pts',(-14.5000018196287,-41.5381172084285,
18.7897579230842));
#16528=CARTESIAN_POINT('Ctrl Pts',(-14.5000187264216,-41.5652595922781,
18.4999999984667));
#16529=CARTESIAN_POINT('Ctrl Pts',(-14.4999998765811,-40.9943207243138,
18.9995579515035));
#16530=CARTESIAN_POINT('Ctrl Pts',(-14.4999999445343,-41.2368464989228,
18.9943613905473));
#16531=CARTESIAN_POINT('Ctrl Pts',(-14.4999999960226,-41.4998332897727,
18.7428715907787));
#16532=CARTESIAN_POINT('Ctrl Pts',(-14.4999999591424,-41.49971461707,18.4999999987146));
#16533=CARTESIAN_POINT('Origin',(0.,0.,23.5));
#16534=CARTESIAN_POINT('Origin',(-15.,13.,14.5));
#16535=CARTESIAN_POINT('',(-19.4370000000001,6.47500000000004,12.5));
#16536=CARTESIAN_POINT('',(-19.437,6.475,14.5));
#16537=CARTESIAN_POINT('',(-19.4370000000002,6.47500000000015,14.5));
#16538=CARTESIAN_POINT('',(-19.5807795062061,6.26355954969803,14.5));
#16539=CARTESIAN_POINT('',(-19.58077950621,6.263559549693,14.5));
#16540=CARTESIAN_POINT('',(-19.5807795062094,6.26355954969258,14.5));
#16541=CARTESIAN_POINT('',(-18.4170000000002,7.97500000000007,14.5));
#16542=CARTESIAN_POINT('',(-15.,13.,14.5));
#16543=CARTESIAN_POINT('',(-18.4170000000001,7.97500000000006,12.5));
#16544=CARTESIAN_POINT('',(-18.4170000000002,7.97500000000011,14.5));
#16545=CARTESIAN_POINT('',(-15.,13.,12.5));
#16546=CARTESIAN_POINT('Origin',(0.,0.,14.5));
#16547=CARTESIAN_POINT('',(-14.5,7.975,14.5));
#16548=CARTESIAN_POINT('',(-14.5,0.,14.5));
#16549=CARTESIAN_POINT('',(0.,7.975,14.5));
#16550=CARTESIAN_POINT('Origin',(-14.5,13.,-20.5));
#16551=CARTESIAN_POINT('',(-14.5,-40.5,12.5));
#16552=CARTESIAN_POINT('',(-14.5,-48.1,12.5));
#16553=CARTESIAN_POINT('',(-14.5,13.,12.5));
#16554=CARTESIAN_POINT('',(-14.5,-48.1,14.5));
#16555=CARTESIAN_POINT('',(-14.5,-48.1,-20.5));
#16556=CARTESIAN_POINT('',(-14.5,-47.8957988313507,14.5));
#16557=CARTESIAN_POINT('',(-14.5,13.,14.5));
#16558=CARTESIAN_POINT('',(-14.5,-21.975,14.5));
#16559=CARTESIAN_POINT('',(-14.5,13.,14.5));
#16560=CARTESIAN_POINT('',(-14.5,-21.975,12.5));
#16561=CARTESIAN_POINT('',(-14.5,-21.975,-20.5));
#16562=CARTESIAN_POINT('',(-14.5000000000001,-18.10025773881,12.5));
#16563=CARTESIAN_POINT('',(-14.5,13.,12.5));
#16564=CARTESIAN_POINT('',(-14.5,-17.89974226119,12.5));
#16565=CARTESIAN_POINT('',(-14.5,13.,12.5));
#16566=CARTESIAN_POINT('',(-14.5,-14.025,12.5));
#16567=CARTESIAN_POINT('',(-14.5,13.,12.5));
#16568=CARTESIAN_POINT('',(-14.5,-14.025,14.5));
#16569=CARTESIAN_POINT('',(-14.5,-14.025,-20.5));
#16570=CARTESIAN_POINT('',(-14.5,0.0250000000000005,14.5));
#16571=CARTESIAN_POINT('',(-14.5,13.,14.5));
#16572=CARTESIAN_POINT('',(-14.5,0.0250000000000005,12.5));
#16573=CARTESIAN_POINT('',(-14.5,0.0250000000000007,-20.5));
#16574=CARTESIAN_POINT('',(-14.4999999999997,3.89974226119284,12.5));
#16575=CARTESIAN_POINT('',(-14.5,13.,12.5));
#16576=CARTESIAN_POINT('',(-14.5,4.100257738807,12.5));
#16577=CARTESIAN_POINT('',(-14.5,13.,12.5));
#16578=CARTESIAN_POINT('',(-14.5,7.975,12.5));
#16579=CARTESIAN_POINT('',(-14.5,13.,12.5));
#16580=CARTESIAN_POINT('',(-14.5,7.975,-20.5));
#16581=CARTESIAN_POINT('',(-14.5,7.975,-14.5));
#16582=CARTESIAN_POINT('',(-14.5,13.,-14.5));
#16583=CARTESIAN_POINT('',(-14.5,7.975,-12.5));
#16584=CARTESIAN_POINT('',(-14.5,7.975,-20.5));
#16585=CARTESIAN_POINT('',(-14.500000000001,4.1002577388064,-12.5));
#16586=CARTESIAN_POINT('',(-14.5,13.,-12.5));
#16587=CARTESIAN_POINT('',(-14.5,3.899742261193,-12.5));
#16588=CARTESIAN_POINT('',(-14.5,13.,-12.5));
#16589=CARTESIAN_POINT('',(-14.5,0.0250000000000004,-12.5));
#16590=CARTESIAN_POINT('',(-14.5,13.,-12.5));
#16591=CARTESIAN_POINT('',(-14.5,0.0250000000000004,-14.5));
#16592=CARTESIAN_POINT('',(-14.5,0.0250000000000007,-20.5));
#16593=CARTESIAN_POINT('',(-14.5,-14.025,-14.5));
#16594=CARTESIAN_POINT('',(-14.5,13.,-14.5));
#16595=CARTESIAN_POINT('',(-14.5,-14.025,-12.5));
#16596=CARTESIAN_POINT('',(-14.5,-14.025,-20.5));
#16597=CARTESIAN_POINT('',(-14.5000000000011,-17.8997422611906,-12.5));
#16598=CARTESIAN_POINT('',(-14.5,13.,-12.5));
#16599=CARTESIAN_POINT('',(-14.5,-18.10025773881,-12.5));
#16600=CARTESIAN_POINT('',(-14.5,13.,-12.5));
#16601=CARTESIAN_POINT('',(-14.5,-21.75,-12.5));
#16602=CARTESIAN_POINT('',(-14.5,13.,-12.5));
#16603=CARTESIAN_POINT('',(-14.5,-21.75,-5.));
#16604=CARTESIAN_POINT('',(-14.5,-21.75,-20.5));
#16605=CARTESIAN_POINT('',(-14.5,-22.475,-5.));
#16606=CARTESIAN_POINT('',(-14.5,0.,-5.));
#16607=CARTESIAN_POINT('',(-14.5,-22.475,12.5));
#16608=CARTESIAN_POINT('',(-14.5,-22.475,-20.5));
#16609=CARTESIAN_POINT('',(-14.5,-38.525,12.5));
#16610=CARTESIAN_POINT('',(-14.5,13.,12.5));
#16611=CARTESIAN_POINT('',(-14.5,-38.525,-5.));
#16612=CARTESIAN_POINT('',(-14.5,-38.525,-20.5));
#16613=CARTESIAN_POINT('',(-14.5,-39.25,-5.));
#16614=CARTESIAN_POINT('',(-14.5,0.,-5.));
#16615=CARTESIAN_POINT('',(-14.5,-39.25,-14.5));
#16616=CARTESIAN_POINT('',(-14.5,-39.25,-20.5));
#16617=CARTESIAN_POINT('',(-14.5,-47.8957988313507,-14.5));
#16618=CARTESIAN_POINT('',(-14.5,13.,-14.5));
#16619=CARTESIAN_POINT('',(-14.5,-48.1,-14.5));
#16620=CARTESIAN_POINT('',(-14.5,13.,-14.5));
#16621=CARTESIAN_POINT('',(-14.5,-48.1,-12.5));
#16622=CARTESIAN_POINT('',(-14.5,-48.1,-20.5));
#16623=CARTESIAN_POINT('',(-14.5,-40.5,-12.5));
#16624=CARTESIAN_POINT('',(-14.5,13.,-12.5));
#16625=CARTESIAN_POINT('',(-14.5,-40.5,-20.5));
#16626=CARTESIAN_POINT('Origin',(0.,0.,-14.5));
#16627=CARTESIAN_POINT('',(-18.4170000000001,7.97500000000004,-14.5));
#16628=CARTESIAN_POINT('',(-15.59525837089,12.12462004281,-14.5));
#16629=CARTESIAN_POINT('',(0.,7.975,-14.5));
#16630=CARTESIAN_POINT('Origin',(-15.,13.,-14.5));
#16631=CARTESIAN_POINT('',(-19.5807795062061,6.26355954969803,-14.5));
#16632=CARTESIAN_POINT('',(-19.437,6.475,-14.5));
#16633=CARTESIAN_POINT('',(-19.58077950621,6.263559549693,-14.5));
#16634=CARTESIAN_POINT('',(-19.4370000000001,6.47500000000004,-12.5));
#16635=CARTESIAN_POINT('',(-19.4370000000002,6.47500000000015,-14.5));
#16636=CARTESIAN_POINT('',(-18.4170000000002,7.97500000000007,-12.5));
#16637=CARTESIAN_POINT('',(-15.,13.,-12.5));
#16638=CARTESIAN_POINT('',(-18.4170000000002,7.97500000000011,-14.5));
#16639=CARTESIAN_POINT('',(-19.5807795062094,6.26355954969258,-14.5));
#16640=CARTESIAN_POINT('Origin',(17.1,4.576629485471,-12.38062237617));
#16641=CARTESIAN_POINT('',(19.5807795062088,6.26355954969267,-14.5));
#16642=CARTESIAN_POINT('',(19.580779506209,6.26355954969229,-12.38062237617));
#16643=CARTESIAN_POINT('',(20.1,4.576629485471,-14.5));
#16644=CARTESIAN_POINT('Origin',(17.1,4.576629485471,-14.5));
#16645=CARTESIAN_POINT('',(20.1,4.576629485471,-12.38062237617));
#16646=CARTESIAN_POINT('Origin',(20.1,-40.6,-14.5));
#16647=CARTESIAN_POINT('',(20.1,1.525,-14.5));
#16648=CARTESIAN_POINT('',(20.1,-40.6,-14.5));
#16649=CARTESIAN_POINT('',(20.1,1.525,-12.5));
#16650=CARTESIAN_POINT('',(20.1,1.525,-14.5));
#16651=CARTESIAN_POINT('',(20.1,0.0249999999999991,-12.5));
#16652=CARTESIAN_POINT('',(20.1,0.,-12.5));
#16653=CARTESIAN_POINT('',(20.1,0.025,-14.5));
#16654=CARTESIAN_POINT('',(20.1,0.0249999999999972,-14.5));
#16655=CARTESIAN_POINT('',(20.1,-14.025,-14.5));
#16656=CARTESIAN_POINT('',(20.1,-40.6,-14.5));
#16657=CARTESIAN_POINT('',(20.1,-14.025,-12.5));
#16658=CARTESIAN_POINT('',(20.1,-14.025,-14.5));
#16659=CARTESIAN_POINT('',(20.1,-15.525,-12.5));
#16660=CARTESIAN_POINT('',(20.1,0.,-12.5));
#16661=CARTESIAN_POINT('',(20.1,-15.525,-14.5));
#16662=CARTESIAN_POINT('',(20.1,-15.525,-14.5));
#16663=CARTESIAN_POINT('',(20.1,-20.475,-14.5));
#16664=CARTESIAN_POINT('',(20.1,-40.6,-14.5));
#16665=CARTESIAN_POINT('',(20.1,-20.475,-12.5));
#16666=CARTESIAN_POINT('',(20.1,-20.475,-14.5));
#16667=CARTESIAN_POINT('',(20.1,-21.975,-12.5));
#16668=CARTESIAN_POINT('',(20.1,0.,-12.5));
#16669=CARTESIAN_POINT('',(20.1,-21.975,-14.5));
#16670=CARTESIAN_POINT('',(20.1,-21.975,-14.5));
#16671=CARTESIAN_POINT('',(20.1,-39.67662948547,-14.5));
#16672=CARTESIAN_POINT('',(20.1,-40.6,-14.5));
#16673=CARTESIAN_POINT('',(20.1,-39.67662948547,-14.5));
#16674=CARTESIAN_POINT('Origin',(17.1,-39.67662948547,-14.38062237617));
#16675=CARTESIAN_POINT('',(19.5807795062097,-41.3635595496912,-14.5));
#16676=CARTESIAN_POINT('Origin',(17.1,-39.67662948547,-14.5));
#16677=CARTESIAN_POINT('',(19.5807795062099,-41.3635595496899,-14.38062237617));
#16678=CARTESIAN_POINT('Origin',(15.,-48.1,-14.5));
#16679=CARTESIAN_POINT('',(15.8928875563296,-46.7869300642212,-14.5));
#16680=CARTESIAN_POINT('',(15.,-48.1,-14.5));
#16681=CARTESIAN_POINT('',(15.8928875563303,-46.7869300642202,-14.5));
#16682=CARTESIAN_POINT('Origin',(13.41210805012,-45.1,-14.36535464022));
#16683=CARTESIAN_POINT('',(14.5,-47.8957988313507,-14.5));
#16684=CARTESIAN_POINT('',(13.4749927141525,-48.0996705000861,-14.5));
#16685=CARTESIAN_POINT('Origin',(13.41210805012,-45.1,-14.5));
#16686=CARTESIAN_POINT('',(13.41210805012,-48.1,-14.5));
#16687=CARTESIAN_POINT('Origin',(13.41210805012,-45.1,-14.5));
#16688=CARTESIAN_POINT('',(13.41210805012,-48.1,-14.36535464022));
#16689=CARTESIAN_POINT('Origin',(13.41210805012,-45.1,-14.5));
#16690=CARTESIAN_POINT('Origin',(-15.,-48.1,-14.5));
#16691=CARTESIAN_POINT('',(8.525,-48.1,-14.5));
#16692=CARTESIAN_POINT('',(-15.,-48.1,-14.5));
#16693=CARTESIAN_POINT('',(8.525,-48.1,-12.5));
#16694=CARTESIAN_POINT('',(8.525,-48.1,-14.5));
#16695=CARTESIAN_POINT('',(7.025,-48.1,-12.5));
#16696=CARTESIAN_POINT('',(0.,-48.1,-12.5));
#16697=CARTESIAN_POINT('',(7.025,-48.1,-14.5));
#16698=CARTESIAN_POINT('',(7.025,-48.1,-14.5));
#16699=CARTESIAN_POINT('',(-7.025,-48.1,-14.5));
#16700=CARTESIAN_POINT('',(-15.,-48.1,-14.5));
#16701=CARTESIAN_POINT('',(-7.025,-48.1,-12.5));
#16702=CARTESIAN_POINT('',(-7.025,-48.1,-14.5));
#16703=CARTESIAN_POINT('',(-8.525,-48.1,-12.5));
#16704=CARTESIAN_POINT('',(0.,-48.1,-12.5));
#16705=CARTESIAN_POINT('',(-8.525,-48.1,-14.5));
#16706=CARTESIAN_POINT('',(-8.525,-48.1,-14.5));
#16707=CARTESIAN_POINT('',(-13.41210805012,-48.1,-14.5));
#16708=CARTESIAN_POINT('',(-15.,-48.1,-14.5));
#16709=CARTESIAN_POINT('',(-13.41210805012,-48.1,-14.5));
#16710=CARTESIAN_POINT('Origin',(-13.41210805012,-45.1,-14.38062237617));
#16711=CARTESIAN_POINT('',(-13.4749927055872,-48.0996705002657,-14.5));
#16712=CARTESIAN_POINT('Origin',(-13.41210805012,-45.1,-14.5));
#16713=CARTESIAN_POINT('',(-15.8928875563293,-46.786930064221,-14.5));
#16714=CARTESIAN_POINT('Origin',(-13.41210805012,-45.1,-14.5));
#16715=CARTESIAN_POINT('',(-15.8928875563299,-46.7869300642199,-14.38062237617));
#16716=CARTESIAN_POINT('Origin',(-13.41210805012,-45.1,-14.5));
#16717=CARTESIAN_POINT('Origin',(-20.1,-40.6,-14.5));
#16718=CARTESIAN_POINT('',(-19.5807795062098,-41.3635595496914,-14.5));
#16719=CARTESIAN_POINT('',(-20.1,-40.6,-14.5));
#16720=CARTESIAN_POINT('',(-19.5807795062105,-41.3635595496904,-14.5));
#16721=CARTESIAN_POINT('Origin',(-17.1,-39.67662948547,-14.36535464022));
#16722=CARTESIAN_POINT('',(-20.1,-39.67662948547,-14.5));
#16723=CARTESIAN_POINT('Origin',(-17.1,-39.67662948547,-14.5));
#16724=CARTESIAN_POINT('',(-20.1,-39.67662948547,-14.36535464022));
#16725=CARTESIAN_POINT('Origin',(-20.1,5.5,-14.5));
#16726=CARTESIAN_POINT('',(-20.1,-21.975,-14.5));
#16727=CARTESIAN_POINT('',(-20.1,5.5,-14.5));
#16728=CARTESIAN_POINT('',(-20.1,-21.975,-12.5));
#16729=CARTESIAN_POINT('',(-20.1,-21.975,-14.5));
#16730=CARTESIAN_POINT('',(-20.1,-20.475,-12.5));
#16731=CARTESIAN_POINT('',(-20.1,5.5,-12.5));
#16732=CARTESIAN_POINT('',(-20.1,-20.475,-14.5));
#16733=CARTESIAN_POINT('',(-20.1,-20.475,-14.5));
#16734=CARTESIAN_POINT('',(-20.1,-15.525,-14.5));
#16735=CARTESIAN_POINT('',(-20.1,5.5,-14.5));
#16736=CARTESIAN_POINT('',(-20.1,-15.525,-12.5));
#16737=CARTESIAN_POINT('',(-20.1,-15.525,-14.5));
#16738=CARTESIAN_POINT('',(-20.1,-14.025,-12.5));
#16739=CARTESIAN_POINT('',(-20.1,5.5,-12.5));
#16740=CARTESIAN_POINT('',(-20.1,-14.025,-14.5));
#16741=CARTESIAN_POINT('',(-20.1,-14.025,-14.5));
#16742=CARTESIAN_POINT('',(-20.1,0.0249999999999999,-14.5));
#16743=CARTESIAN_POINT('',(-20.1,5.5,-14.5));
#16744=CARTESIAN_POINT('',(-20.1,0.0249999999999999,-12.5));
#16745=CARTESIAN_POINT('',(-20.1,0.0249999999999998,-14.5));
#16746=CARTESIAN_POINT('',(-20.1,1.525,-12.5));
#16747=CARTESIAN_POINT('',(-20.1,5.5,-12.5));
#16748=CARTESIAN_POINT('',(-20.1,1.525,-14.5));
#16749=CARTESIAN_POINT('',(-20.1,1.525,-14.5));
#16750=CARTESIAN_POINT('',(-20.1,4.576629485471,-14.5));
#16751=CARTESIAN_POINT('',(-20.1,5.5,-14.5));
#16752=CARTESIAN_POINT('',(-20.1,4.576629485471,-14.5));
#16753=CARTESIAN_POINT('Origin',(-17.1,4.576629485471,-12.38062237617));
#16754=CARTESIAN_POINT('Origin',(-17.1,4.576629485471,-14.5));
#16755=CARTESIAN_POINT('Origin',(-6.64999999999998,9.49999999999996,-17.));
#16756=CARTESIAN_POINT('',(-8.15,9.5,-19.));
#16757=CARTESIAN_POINT('Origin',(-6.65,9.5,-19.));
#16758=CARTESIAN_POINT('Origin',(-8.15,9.49999999999999,-17.));
#16759=CARTESIAN_POINT('Origin',(-8.15,13.,-20.5));
#16760=CARTESIAN_POINT('',(-8.15,9.00000000030975,-19.));
#16761=CARTESIAN_POINT('',(-8.15,13.,-19.));
#16762=CARTESIAN_POINT('',(-8.15,9.,-20.5));
#16763=CARTESIAN_POINT('Origin',(-10.5,9.,-20.5));
#16764=CARTESIAN_POINT('',(-10.5,6.65,-19.));
#16765=CARTESIAN_POINT('',(-10.5,6.65,-20.5));
#16766=CARTESIAN_POINT('Origin',(-10.5,9.,-19.));
#16767=CARTESIAN_POINT('Origin',(-10.5,6.65,-20.5));
#16768=CARTESIAN_POINT('',(-13.5,6.6500000000001,-18.4999999994861));
#16769=CARTESIAN_POINT('',(-13.,6.65000000000009,-18.9999999999985));
#16770=CARTESIAN_POINT('Ctrl Pts',(-13.5,6.65000000000025,-18.4999999994861));
#16771=CARTESIAN_POINT('Ctrl Pts',(-13.5000000003688,6.65000000000034,-18.7411872045822));
#16772=CARTESIAN_POINT('Ctrl Pts',(-13.2411750364478,6.65000000000035,-18.9975772517629));
#16773=CARTESIAN_POINT('Ctrl Pts',(-13.,6.65000000000028,-18.9999999999985));
#16774=CARTESIAN_POINT('',(-13.5,6.65,-20.5));
#16775=CARTESIAN_POINT('',(-10.5,6.65,-19.));
#16776=CARTESIAN_POINT('Origin',(-13.5,5.65,-16.88062237617));
#16777=CARTESIAN_POINT('',(-14.4999999999994,5.65,-18.4999999994854));
#16778=CARTESIAN_POINT('Origin',(-13.5000000000004,5.65000000000104,-18.5000000058401));
#16779=CARTESIAN_POINT('',(-14.5,5.65,-16.88062237617));
#16780=CARTESIAN_POINT('Origin',(-14.5,13.,-20.5));
#16781=CARTESIAN_POINT('',(-14.5000000000002,5.14999999999998,-18.9999999999996));
#16782=CARTESIAN_POINT('Ctrl Pts',(-14.5000000000005,5.14999999999998,-18.9999999999996));
#16783=CARTESIAN_POINT('Ctrl Pts',(-14.5000000000009,5.39101397566289,-18.9908604458716));
#16784=CARTESIAN_POINT('Ctrl Pts',(-14.4999999999995,5.65000000036765,-18.7411872045961));
#16785=CARTESIAN_POINT('Ctrl Pts',(-14.4999999999986,5.65,-18.4999999994854));
#16786=CARTESIAN_POINT('',(-14.5000000000004,-34.65,-18.9999999999984));
#16787=CARTESIAN_POINT('',(-14.5,13.,-19.));
#16788=CARTESIAN_POINT('',(-14.5000000000008,-35.15,-18.4999999994855));
#16789=CARTESIAN_POINT('Ctrl Pts',(-14.5000000000019,-35.15,-18.4999999994855));
#16790=CARTESIAN_POINT('Ctrl Pts',(-14.5000000000027,-35.1500000003693,
-18.7411872045814));
#16791=CARTESIAN_POINT('Ctrl Pts',(-14.5000000000008,-34.891175036448,-18.9975772517615));
#16792=CARTESIAN_POINT('Ctrl Pts',(-14.5000000000013,-34.65,-18.9999999999984));
#16793=CARTESIAN_POINT('',(-14.5,-35.15,-20.5));
#16794=CARTESIAN_POINT('Origin',(-13.5,-35.15,-20.63464535978));
#16795=CARTESIAN_POINT('',(-13.4999999999999,-36.1499999999995,-18.4999999994848));
#16796=CARTESIAN_POINT('Origin',(-13.4999999999957,-35.1499999999943,-18.500000005847));
#16797=CARTESIAN_POINT('',(-13.5,-36.15,-20.63464535978));
#16798=CARTESIAN_POINT('Origin',(-14.5,-36.15,-20.5));
#16799=CARTESIAN_POINT('',(-10.5,-36.15,-19.));
#16800=CARTESIAN_POINT('',(-10.5,-36.15,-20.5));
#16801=CARTESIAN_POINT('',(-13.,-36.1500000000002,-19.));
#16802=CARTESIAN_POINT('Ctrl Pts',(-13.,-36.1500000000006,-19.));
#16803=CARTESIAN_POINT('Ctrl Pts',(-13.2410139756646,-36.1500000000009,
-18.9908604458711));
#16804=CARTESIAN_POINT('Ctrl Pts',(-13.5000000003674,-36.1499999999995,
-18.7411872045957));
#16805=CARTESIAN_POINT('Ctrl Pts',(-13.4999999999999,-36.1499999999986,
-18.4999999994848));
#16806=CARTESIAN_POINT('',(-14.5,-36.15,-19.));
#16807=CARTESIAN_POINT('Origin',(-10.5,-38.5,-20.5));
#16808=CARTESIAN_POINT('',(-8.15,-38.5000000003124,-19.));
#16809=CARTESIAN_POINT('',(-8.15,-38.5,-20.5));
#16810=CARTESIAN_POINT('Origin',(-10.5,-38.5,-19.));
#16811=CARTESIAN_POINT('Origin',(-8.15,-38.5,-20.5));
#16812=CARTESIAN_POINT('',(-8.1500000000001,-41.5,-18.4999999994855));
#16813=CARTESIAN_POINT('',(-8.14999999999996,-41.,-18.9999999999984));
#16814=CARTESIAN_POINT('Ctrl Pts',(-8.15000000000025,-41.5,-18.4999999994855));
#16815=CARTESIAN_POINT('Ctrl Pts',(-8.15000000000033,-41.5000000003692,
-18.7411872045814));
#16816=CARTESIAN_POINT('Ctrl Pts',(-8.1500000000003,-41.241175036448,-18.9975772517615));
#16817=CARTESIAN_POINT('Ctrl Pts',(-8.14999999999988,-41.,-18.9999999999984));
#16818=CARTESIAN_POINT('',(-8.15,-41.5,-20.5));
#16819=CARTESIAN_POINT('',(-8.15,-38.5,-19.));
#16820=CARTESIAN_POINT('Origin',(-7.15,-41.5,-16.88062237617));
#16821=CARTESIAN_POINT('',(-7.15,-42.4999999999995,-18.4999999994848));
#16822=CARTESIAN_POINT('Origin',(-7.15000000000103,-41.5000000000004,-18.500000005847));
#16823=CARTESIAN_POINT('',(-7.15,-42.5,-16.88062237617));
#16824=CARTESIAN_POINT('Origin',(-14.5,-42.5,-20.5));
#16825=CARTESIAN_POINT('',(-6.64999999999998,-42.5000000000002,-18.9999999999996));
#16826=CARTESIAN_POINT('Ctrl Pts',(-6.64999999999998,-42.5000000000005,
-18.9999999999996));
#16827=CARTESIAN_POINT('Ctrl Pts',(-6.89101397566309,-42.5000000000009,
-18.9908604458716));
#16828=CARTESIAN_POINT('Ctrl Pts',(-7.15000000036808,-42.4999999999995,
-18.7411872045957));
#16829=CARTESIAN_POINT('Ctrl Pts',(-7.15,-42.4999999999986,-18.4999999994848));
#16830=CARTESIAN_POINT('',(6.65,-42.5000000000004,-19.));
#16831=CARTESIAN_POINT('',(-14.5,-42.5,-19.));
#16832=CARTESIAN_POINT('',(7.15,-42.5000000000008,-18.4999999994861));
#16833=CARTESIAN_POINT('Ctrl Pts',(7.15,-42.5000000000019,-18.4999999994861));
#16834=CARTESIAN_POINT('Ctrl Pts',(7.15000000036776,-42.5000000000027,-18.7411872045842));
#16835=CARTESIAN_POINT('Ctrl Pts',(6.89117503644782,-42.5000000000008,-18.997577251766));
#16836=CARTESIAN_POINT('Ctrl Pts',(6.65,-42.5000000000013,-19.));
#16837=CARTESIAN_POINT('',(7.15,-42.5,-20.5));
#16838=CARTESIAN_POINT('Origin',(7.15,-41.5,-20.63464535978));
#16839=CARTESIAN_POINT('',(8.15000000000002,-41.4999999999999,-18.4999999994854));
#16840=CARTESIAN_POINT('Origin',(7.149999999994,-41.4999999999948,-18.5000000058402));
#16841=CARTESIAN_POINT('',(8.15,-41.5,-20.63464535978));
#16842=CARTESIAN_POINT('Origin',(8.15,-42.5,-20.5));
#16843=CARTESIAN_POINT('',(8.15,-38.5,-19.));
#16844=CARTESIAN_POINT('',(8.15,-38.5,-20.5));
#16845=CARTESIAN_POINT('',(8.15,-41.,-19.));
#16846=CARTESIAN_POINT('Ctrl Pts',(8.14999999999999,-41.,-19.));
#16847=CARTESIAN_POINT('Ctrl Pts',(8.15000000000028,-41.2410139756644,-18.9908604458711));
#16848=CARTESIAN_POINT('Ctrl Pts',(8.15000000000017,-41.5000000003669,-18.7411872045961));
#16849=CARTESIAN_POINT('Ctrl Pts',(8.15000000000004,-41.5,-18.4999999994854));
#16850=CARTESIAN_POINT('',(8.15,-42.5,-19.));
#16851=CARTESIAN_POINT('Origin',(10.5,-38.5,-20.5));
#16852=CARTESIAN_POINT('',(10.5000000003124,-36.15,-19.));
#16853=CARTESIAN_POINT('',(10.5,-36.15,-20.5));
#16854=CARTESIAN_POINT('Origin',(10.5,-38.5,-19.));
#16855=CARTESIAN_POINT('Origin',(10.5,-36.15,-20.5));
#16856=CARTESIAN_POINT('',(13.5,-36.1500000000008,-18.4999999994861));
#16857=CARTESIAN_POINT('',(13.,-36.1500000000004,-18.9999999999985));
#16858=CARTESIAN_POINT('Ctrl Pts',(13.5,-36.1500000000019,-18.4999999994861));
#16859=CARTESIAN_POINT('Ctrl Pts',(13.5000000003688,-36.1500000000027,-18.7411872045822));
#16860=CARTESIAN_POINT('Ctrl Pts',(13.2411750364478,-36.1500000000008,-18.9975772517629));
#16861=CARTESIAN_POINT('Ctrl Pts',(13.,-36.1500000000013,-18.9999999999985));
#16862=CARTESIAN_POINT('',(13.5,-36.15,-20.5));
#16863=CARTESIAN_POINT('',(10.5,-36.15,-19.));
#16864=CARTESIAN_POINT('Origin',(13.5,-35.15,-16.88062237617));
#16865=CARTESIAN_POINT('',(14.4999999999994,-35.1499999999999,-18.4999999994854));
#16866=CARTESIAN_POINT('Origin',(13.4999999999943,-35.1499999999957,-18.5000000058401));
#16867=CARTESIAN_POINT('',(14.5,-35.15,-16.88062237617));
#16868=CARTESIAN_POINT('Origin',(14.5,-42.5,-20.5));
#16869=CARTESIAN_POINT('',(14.5000000000002,-34.65,-19.));
#16870=CARTESIAN_POINT('Ctrl Pts',(14.5000000000005,-34.65,-19.));
#16871=CARTESIAN_POINT('Ctrl Pts',(14.5000000000009,-34.8910139756644,-18.9908604458711));
#16872=CARTESIAN_POINT('Ctrl Pts',(14.4999999999995,-35.1500000003669,-18.7411872045961));
#16873=CARTESIAN_POINT('Ctrl Pts',(14.4999999999986,-35.1499999999999,-18.4999999994854));
#16874=CARTESIAN_POINT('',(14.5000000000004,5.15,-18.9999999999998));
#16875=CARTESIAN_POINT('',(14.5,-42.5,-19.));
#16876=CARTESIAN_POINT('',(14.5000000000008,5.65,-18.4999999994855));
#16877=CARTESIAN_POINT('Ctrl Pts',(14.5000000000019,5.65,-18.4999999994855));
#16878=CARTESIAN_POINT('Ctrl Pts',(14.5000000000027,5.65000000036822,-18.7411872045835));
#16879=CARTESIAN_POINT('Ctrl Pts',(14.5000000000008,5.39117503644798,-18.9975772517647));
#16880=CARTESIAN_POINT('Ctrl Pts',(14.5000000000013,5.15,-18.9999999999998));
#16881=CARTESIAN_POINT('',(14.5,5.65,-20.5));
#16882=CARTESIAN_POINT('Origin',(13.5,5.65,-20.63464535978));
#16883=CARTESIAN_POINT('',(13.4999999999999,6.65000000000002,-18.4999999994848));
#16884=CARTESIAN_POINT('Origin',(13.4999999999948,5.649999999994,-18.500000005847));
#16885=CARTESIAN_POINT('',(13.5,6.65,-20.63464535978));
#16886=CARTESIAN_POINT('Origin',(14.5,6.65,-20.5));
#16887=CARTESIAN_POINT('',(10.5,6.65,-19.));
#16888=CARTESIAN_POINT('',(10.5,6.65,-20.5));
#16889=CARTESIAN_POINT('',(13.,6.65,-19.));
#16890=CARTESIAN_POINT('Ctrl Pts',(13.,6.64999999999999,-19.));
#16891=CARTESIAN_POINT('Ctrl Pts',(13.2410139756646,6.65000000000028,-18.9908604458711));
#16892=CARTESIAN_POINT('Ctrl Pts',(13.5000000003674,6.65000000000017,-18.7411872045957));
#16893=CARTESIAN_POINT('Ctrl Pts',(13.4999999999999,6.65000000000004,-18.4999999994848));
#16894=CARTESIAN_POINT('',(14.5,6.65,-19.));
#16895=CARTESIAN_POINT('Origin',(10.5,9.,-20.5));
#16896=CARTESIAN_POINT('',(8.15,9.000000000459,-19.));
#16897=CARTESIAN_POINT('',(8.15,9.000000000918,-20.5));
#16898=CARTESIAN_POINT('Origin',(10.5,9.,-19.));
#16899=CARTESIAN_POINT('Origin',(8.15,9.,-20.5));
#16900=CARTESIAN_POINT('',(8.15,9.5,-19.));
#16901=CARTESIAN_POINT('',(8.15,9.639713176691,-19.));
#16902=CARTESIAN_POINT('Origin',(8.15,9.49999999999999,-17.));
#16903=CARTESIAN_POINT('Origin',(6.65,9.50000000000007,-17.0000000000001));
#16904=CARTESIAN_POINT('Origin',(6.65,9.5,-19.));
#16905=CARTESIAN_POINT('Origin',(20.1,5.5,-14.5));
#16906=CARTESIAN_POINT('',(18.4169999999999,7.97499999999996,-14.5));
#16907=CARTESIAN_POINT('',(20.1,5.5,-14.5));
#16908=CARTESIAN_POINT('',(18.4169999999999,7.97499999999996,-12.5));
#16909=CARTESIAN_POINT('',(18.4169999999999,7.97499999999994,-14.5));
#16910=CARTESIAN_POINT('',(19.437,6.47499999999999,-12.5));
#16911=CARTESIAN_POINT('',(20.1,5.5,-12.5));
#16912=CARTESIAN_POINT('',(19.437,6.47499999999999,-14.5));
#16913=CARTESIAN_POINT('',(19.437,6.47499999999998,-14.5));
#16914=CARTESIAN_POINT('',(20.1,5.5,-14.5));
#16915=CARTESIAN_POINT('Origin',(0.,0.,-20.5));
#16916=CARTESIAN_POINT('',(10.5000000000002,5.1500005893432,-20.4999999999999));
#16917=CARTESIAN_POINT('',(6.65000039306064,9.00000000001898,-20.4999999999998));
#16918=CARTESIAN_POINT('Origin',(10.5000016830354,9.0000020756571,-20.5000000000012));
#16919=CARTESIAN_POINT('',(13.,5.15,-20.5));
#16920=CARTESIAN_POINT('',(0.,5.15,-20.5));
#16921=CARTESIAN_POINT('',(13.,-34.65000000018,-20.5));
#16922=CARTESIAN_POINT('',(13.,0.,-20.5));
#16923=CARTESIAN_POINT('',(10.5000000005402,-34.6500004912993,-20.4999999999998));
#16924=CARTESIAN_POINT('',(0.,-34.65000000024,-20.5));
#16925=CARTESIAN_POINT('',(6.6500005893432,-38.5000000000002,-20.4999999999999));
#16926=CARTESIAN_POINT('Origin',(10.5000017894248,-38.5000015931868,-20.500000000001));
#16927=CARTESIAN_POINT('',(6.65,-41.,-20.5));
#16928=CARTESIAN_POINT('',(6.65,0.,-20.5));
#16929=CARTESIAN_POINT('',(-6.650000000177,-41.,-20.5));
#16930=CARTESIAN_POINT('',(0.,-41.,-20.5));
#16931=CARTESIAN_POINT('',(-6.65000049129643,-38.5000000005401,-20.4999999999998));
#16932=CARTESIAN_POINT('',(-6.650000000236,0.,-20.5));
#16933=CARTESIAN_POINT('',(-10.4999999999999,-34.6500012274245,-20.4999999999997));
#16934=CARTESIAN_POINT('Origin',(-10.4999997334424,-38.5000012060096,-20.5000000000009));
#16935=CARTESIAN_POINT('',(-13.,-34.65,-20.5));
#16936=CARTESIAN_POINT('',(0.,-34.65,-20.5));
#16937=CARTESIAN_POINT('',(-13.,5.1500019635795,-20.5));
#16938=CARTESIAN_POINT('',(-13.,0.,-20.5));
#16939=CARTESIAN_POINT('',(-10.5000000000006,5.15000274884423,-20.4999999999992));
#16940=CARTESIAN_POINT('',(0.,5.150003927159,-20.5));
#16941=CARTESIAN_POINT('',(-6.65000000007813,9.00000000072159,-20.5));
#16942=CARTESIAN_POINT('Origin',(-10.499997711063,8.99999928187284,-20.5));
#16943=CARTESIAN_POINT('',(-6.65,0.,-20.5));
#16944=CARTESIAN_POINT('',(6.650000000236,0.,-20.5));
#16945=CARTESIAN_POINT('Origin',(0.,0.,-14.5));
#16946=CARTESIAN_POINT('',(14.5,7.975,-14.5));
#16947=CARTESIAN_POINT('',(0.,7.975,-14.5));
#16948=CARTESIAN_POINT('',(14.5,0.,-14.5));
#16949=CARTESIAN_POINT('Origin',(0.,0.,14.5));
#16950=CARTESIAN_POINT('',(18.417,7.97499999999998,14.5));
#16951=CARTESIAN_POINT('',(18.417,7.975,14.5));
#16952=CARTESIAN_POINT('',(14.5,7.975,14.5));
#16953=CARTESIAN_POINT('',(0.,7.975,14.5));
#16954=CARTESIAN_POINT('',(14.5,0.,14.5));
#16955=CARTESIAN_POINT('Origin',(14.5,-42.5,-20.5));
#16956=CARTESIAN_POINT('',(14.5,-21.975,12.5));
#16957=CARTESIAN_POINT('',(14.5,-21.975,14.5));
#16958=CARTESIAN_POINT('',(14.5,-21.975,-20.5));
#16959=CARTESIAN_POINT('',(14.5,-47.8957988313507,14.5));
#16960=CARTESIAN_POINT('',(14.5,-42.5,14.5));
#16961=CARTESIAN_POINT('',(14.5,-48.1,14.5));
#16962=CARTESIAN_POINT('',(14.5,-42.5,14.5));
#16963=CARTESIAN_POINT('',(14.5,-48.1,12.5));
#16964=CARTESIAN_POINT('',(14.5,-48.1,-20.5));
#16965=CARTESIAN_POINT('',(14.5,-40.5,12.5));
#16966=CARTESIAN_POINT('',(14.5,-42.5,12.5));
#16967=CARTESIAN_POINT('',(14.5,-40.5,-12.5));
#16968=CARTESIAN_POINT('',(14.5,-40.5,-20.5));
#16969=CARTESIAN_POINT('',(14.5,-48.1,-12.5));
#16970=CARTESIAN_POINT('',(14.5,-42.5,-12.5));
#16971=CARTESIAN_POINT('',(14.5,-48.1,-14.5));
#16972=CARTESIAN_POINT('',(14.5,-48.1,-20.5));
#16973=CARTESIAN_POINT('',(14.5,-42.5,-14.5));
#16974=CARTESIAN_POINT('',(14.5,-39.25,-14.5));
#16975=CARTESIAN_POINT('',(14.5,-42.5,-14.5));
#16976=CARTESIAN_POINT('',(14.5,-39.25,-5.));
#16977=CARTESIAN_POINT('',(14.5,-39.25,-20.5));
#16978=CARTESIAN_POINT('',(14.5,-38.525,-5.));
#16979=CARTESIAN_POINT('',(14.5,0.,-5.));
#16980=CARTESIAN_POINT('',(14.5,-38.525,12.5));
#16981=CARTESIAN_POINT('',(14.5,-38.525,-20.5));
#16982=CARTESIAN_POINT('',(14.5,-22.475,12.5));
#16983=CARTESIAN_POINT('',(14.5,-42.5,12.5));
#16984=CARTESIAN_POINT('',(14.5,-22.475,-5.));
#16985=CARTESIAN_POINT('',(14.5,-22.475,-20.5));
#16986=CARTESIAN_POINT('',(14.5,-21.75,-5.));
#16987=CARTESIAN_POINT('',(14.5,0.,-5.));
#16988=CARTESIAN_POINT('',(14.5,-21.75,-12.5));
#16989=CARTESIAN_POINT('',(14.5,-21.75,-20.5));
#16990=CARTESIAN_POINT('',(14.5,-18.10025773881,-12.5));
#16991=CARTESIAN_POINT('',(14.5,-42.5,-12.5));
#16992=CARTESIAN_POINT('',(14.5,-17.89974226119,-12.5));
#16993=CARTESIAN_POINT('',(14.5,-42.5,-12.5));
#16994=CARTESIAN_POINT('',(14.5,-14.025,-12.5));
#16995=CARTESIAN_POINT('',(14.5,-42.5,-12.5));
#16996=CARTESIAN_POINT('',(14.5,-14.025,-14.5));
#16997=CARTESIAN_POINT('',(14.5,-14.025,-20.5));
#16998=CARTESIAN_POINT('',(14.5,0.0249999999999982,-14.5));
#16999=CARTESIAN_POINT('',(14.5,-42.5,-14.5));
#17000=CARTESIAN_POINT('',(14.5,0.0249999999999982,-12.5));
#17001=CARTESIAN_POINT('',(14.5,0.0249999999999972,-20.5));
#17002=CARTESIAN_POINT('',(14.5,3.899742261193,-12.5));
#17003=CARTESIAN_POINT('',(14.5,-42.5,-12.5));
#17004=CARTESIAN_POINT('',(14.5,4.100257738807,-12.5));
#17005=CARTESIAN_POINT('',(14.5,-42.5,-12.5));
#17006=CARTESIAN_POINT('',(14.5,7.975,-12.5));
#17007=CARTESIAN_POINT('',(14.5,-42.5,-12.5));
#17008=CARTESIAN_POINT('',(14.5,7.975,-20.5));
#17009=CARTESIAN_POINT('',(14.5,7.975,12.5));
#17010=CARTESIAN_POINT('',(14.5,7.975,-20.5));
#17011=CARTESIAN_POINT('',(14.4999999999997,4.10025773880716,12.5));
#17012=CARTESIAN_POINT('',(14.5,-42.5,12.5));
#17013=CARTESIAN_POINT('',(14.5,3.899742261193,12.5));
#17014=CARTESIAN_POINT('',(14.5,-42.5,12.5));
#17015=CARTESIAN_POINT('',(14.5,0.0249999999999982,12.5));
#17016=CARTESIAN_POINT('',(14.5,-42.5,12.5));
#17017=CARTESIAN_POINT('',(14.5,0.0249999999999982,14.5));
#17018=CARTESIAN_POINT('',(14.5,0.0249999999999972,-20.5));
#17019=CARTESIAN_POINT('',(14.5,-14.025,14.5));
#17020=CARTESIAN_POINT('',(14.5,-42.5,14.5));
#17021=CARTESIAN_POINT('',(14.5,-14.025,12.5));
#17022=CARTESIAN_POINT('',(14.5,-14.025,-20.5));
#17023=CARTESIAN_POINT('',(14.5000000000001,-17.89974226119,12.5));
#17024=CARTESIAN_POINT('',(14.5,-42.5,12.5));
#17025=CARTESIAN_POINT('',(14.5,-18.10025773881,12.5));
#17026=CARTESIAN_POINT('',(14.5,-42.5,12.5));
#17027=CARTESIAN_POINT('',(14.5,-42.5,12.5));
#17028=CARTESIAN_POINT('Origin',(20.1,5.5,14.5));
#17029=CARTESIAN_POINT('',(19.580779506206,6.26355954969795,14.5));
#17030=CARTESIAN_POINT('',(19.5807795062091,6.26355954969241,14.5));
#17031=CARTESIAN_POINT('',(19.437,6.47499999999999,14.5));
#17032=CARTESIAN_POINT('',(19.437,6.475,14.5));
#17033=CARTESIAN_POINT('',(19.437,6.47499999999999,12.5));
#17034=CARTESIAN_POINT('',(19.437,6.47499999999998,14.5));
#17035=CARTESIAN_POINT('',(18.417,7.97499999999996,12.5));
#17036=CARTESIAN_POINT('',(20.1,5.5,12.5));
#17037=CARTESIAN_POINT('',(18.4169999999999,7.97499999999994,14.5));
#17038=CARTESIAN_POINT('Origin',(20.1,-40.6,14.5));
#17039=CARTESIAN_POINT('',(20.1,1.525,12.5));
#17040=CARTESIAN_POINT('',(20.1,1.525,14.5));
#17041=CARTESIAN_POINT('',(20.1,1.525,14.5));
#17042=CARTESIAN_POINT('',(20.1,4.576629485471,14.5));
#17043=CARTESIAN_POINT('',(20.1,-40.6,14.5));
#17044=CARTESIAN_POINT('',(20.1,4.576629485471,14.5));
#17045=CARTESIAN_POINT('',(20.1,-39.67662948547,14.5));
#17046=CARTESIAN_POINT('',(20.1,-39.67662948547,14.5));
#17047=CARTESIAN_POINT('',(20.1,-21.975,14.5));
#17048=CARTESIAN_POINT('',(20.1,-40.6,14.5));
#17049=CARTESIAN_POINT('',(20.1,-21.975,12.5));
#17050=CARTESIAN_POINT('',(20.1,-21.975,14.5));
#17051=CARTESIAN_POINT('',(20.1,-20.475,12.5));
#17052=CARTESIAN_POINT('',(20.1,-40.6,12.5));
#17053=CARTESIAN_POINT('',(20.1,-20.475,14.5));
#17054=CARTESIAN_POINT('',(20.1,-20.475,14.5));
#17055=CARTESIAN_POINT('',(20.1,-15.525,14.5));
#17056=CARTESIAN_POINT('',(20.1,-40.6,14.5));
#17057=CARTESIAN_POINT('',(20.1,-15.525,12.5));
#17058=CARTESIAN_POINT('',(20.1,-15.525,14.5));
#17059=CARTESIAN_POINT('',(20.1,-14.025,12.5));
#17060=CARTESIAN_POINT('',(20.1,-40.6,12.5));
#17061=CARTESIAN_POINT('',(20.1,-14.025,14.5));
#17062=CARTESIAN_POINT('',(20.1,-14.025,14.5));
#17063=CARTESIAN_POINT('',(20.1,0.0249999999999982,14.5));
#17064=CARTESIAN_POINT('',(20.1,-40.6,14.5));
#17065=CARTESIAN_POINT('',(20.1,0.0249999999999982,12.5));
#17066=CARTESIAN_POINT('',(20.1,0.0249999999999972,14.5));
#17067=CARTESIAN_POINT('',(20.1,-40.6,12.5));
#17068=CARTESIAN_POINT('Origin',(17.1,-39.67662948547,17.13971317669));
#17069=CARTESIAN_POINT('',(19.5807795062097,-41.3635595496912,14.5));
#17070=CARTESIAN_POINT('',(19.5807795062099,-41.3635595496899,17.13971317669));
#17071=CARTESIAN_POINT('Origin',(17.1,-39.67662948547,14.5));
#17072=CARTESIAN_POINT('Origin',(15.,-48.1,14.5));
#17073=CARTESIAN_POINT('',(15.8928875563296,-46.7869300642212,14.5));
#17074=CARTESIAN_POINT('',(15.8928875563303,-46.7869300642202,14.5));
#17075=CARTESIAN_POINT('',(15.,-48.1,14.5));
#17076=CARTESIAN_POINT('Origin',(13.41210805012,-45.1,17.13971317669));
#17077=CARTESIAN_POINT('',(13.41210805012,-48.1,14.5));
#17078=CARTESIAN_POINT('',(13.41210805012,-48.1,17.13971317669));
#17079=CARTESIAN_POINT('',(13.4749927054462,-48.0996705002687,14.5));
#17080=CARTESIAN_POINT('Origin',(13.41210805012,-45.1,14.5));
#17081=CARTESIAN_POINT('Origin',(13.41210805012,-45.1,14.5));
#17082=CARTESIAN_POINT('Origin',(13.41210805012,-45.1,14.5));
#17083=CARTESIAN_POINT('Origin',(-15.,-48.1,14.5));
#17084=CARTESIAN_POINT('',(8.525,-48.1,12.5));
#17085=CARTESIAN_POINT('',(8.525,-48.1,14.5));
#17086=CARTESIAN_POINT('',(8.525,-48.1,14.5));
#17087=CARTESIAN_POINT('',(-15.,-48.1,14.5));
#17088=CARTESIAN_POINT('',(-13.41210805012,-48.1,14.5));
#17089=CARTESIAN_POINT('',(-13.41210805012,-48.1,14.5));
#17090=CARTESIAN_POINT('',(-8.525,-48.1,14.5));
#17091=CARTESIAN_POINT('',(-15.,-48.1,14.5));
#17092=CARTESIAN_POINT('',(-8.525,-48.1,12.5));
#17093=CARTESIAN_POINT('',(-8.525,-48.1,14.5));
#17094=CARTESIAN_POINT('',(-7.025,-48.1,12.5));
#17095=CARTESIAN_POINT('',(0.,-48.1,12.5));
#17096=CARTESIAN_POINT('',(-7.025,-48.1,14.5));
#17097=CARTESIAN_POINT('',(-7.025,-48.1,14.5));
#17098=CARTESIAN_POINT('',(7.025,-48.1,14.5));
#17099=CARTESIAN_POINT('',(-15.,-48.1,14.5));
#17100=CARTESIAN_POINT('',(7.025,-48.1,12.5));
#17101=CARTESIAN_POINT('',(7.025,-48.1,14.5));
#17102=CARTESIAN_POINT('',(0.,-48.1,12.5));
#17103=CARTESIAN_POINT('Origin',(-13.41210805012,-45.1,17.13971317669));
#17104=CARTESIAN_POINT('',(-15.8928875563293,-46.786930064221,14.5));
#17105=CARTESIAN_POINT('',(-15.8928875563299,-46.7869300642199,17.13971317669));
#17106=CARTESIAN_POINT('Origin',(-13.41210805012,-45.1,14.5));
#17107=CARTESIAN_POINT('',(-13.4749927055872,-48.0996705002657,14.5));
#17108=CARTESIAN_POINT('Origin',(-13.41210805012,-45.1,14.5));
#17109=CARTESIAN_POINT('Origin',(-13.41210805012,-45.1,14.5));
#17110=CARTESIAN_POINT('Origin',(-20.1,-40.6,14.5));
#17111=CARTESIAN_POINT('',(-19.5807795062098,-41.3635595496914,14.5));
#17112=CARTESIAN_POINT('',(-19.5807795062105,-41.3635595496904,14.5));
#17113=CARTESIAN_POINT('',(-20.1,-40.6,14.5));
#17114=CARTESIAN_POINT('Origin',(-17.1,-39.67662948547,17.13971317669));
#17115=CARTESIAN_POINT('',(-20.1,-39.67662948547,14.5));
#17116=CARTESIAN_POINT('',(-20.1,-39.67662948547,17.13971317669));
#17117=CARTESIAN_POINT('Origin',(-17.1,-39.67662948547,14.5));
#17118=CARTESIAN_POINT('Origin',(-20.1,5.5,14.5));
#17119=CARTESIAN_POINT('',(-20.1,-21.975,12.5));
#17120=CARTESIAN_POINT('',(-20.1,-21.975,14.5));
#17121=CARTESIAN_POINT('',(-20.1,-21.975,14.5));
#17122=CARTESIAN_POINT('',(-20.1,5.5,14.5));
#17123=CARTESIAN_POINT('',(-20.1,4.576629485471,14.5));
#17124=CARTESIAN_POINT('',(-20.1,4.576629485471,14.5));
#17125=CARTESIAN_POINT('',(-20.1,1.525,14.5));
#17126=CARTESIAN_POINT('',(-20.1,5.5,14.5));
#17127=CARTESIAN_POINT('',(-20.1,1.525,12.5));
#17128=CARTESIAN_POINT('',(-20.1,1.525,14.5));
#17129=CARTESIAN_POINT('',(-20.1,0.0249999999999999,12.5));
#17130=CARTESIAN_POINT('',(-20.1,5.5,12.5));
#17131=CARTESIAN_POINT('',(-20.1,0.0249999999999999,14.5));
#17132=CARTESIAN_POINT('',(-20.1,0.0249999999999998,14.5));
#17133=CARTESIAN_POINT('',(-20.1,-14.025,14.5));
#17134=CARTESIAN_POINT('',(-20.1,5.5,14.5));
#17135=CARTESIAN_POINT('',(-20.1,-14.025,12.5));
#17136=CARTESIAN_POINT('',(-20.1,-14.025,14.5));
#17137=CARTESIAN_POINT('',(-20.1,-15.525,12.5));
#17138=CARTESIAN_POINT('',(-20.1,5.5,12.5));
#17139=CARTESIAN_POINT('',(-20.1,-15.525,14.5));
#17140=CARTESIAN_POINT('',(-20.1,-15.525,14.5));
#17141=CARTESIAN_POINT('',(-20.1,-20.475,14.5));
#17142=CARTESIAN_POINT('',(-20.1,5.5,14.5));
#17143=CARTESIAN_POINT('',(-20.1,-20.475,12.5));
#17144=CARTESIAN_POINT('',(-20.1,-20.475,14.5));
#17145=CARTESIAN_POINT('',(-20.1,5.5,12.5));
#17146=CARTESIAN_POINT('Origin',(-17.1,4.576629485471,17.13971317669));
#17147=CARTESIAN_POINT('Origin',(-17.1,4.576629485471,14.5));
#17148=CARTESIAN_POINT('Origin',(17.1,4.576629485471,17.13971317669));
#17149=CARTESIAN_POINT('Origin',(17.1,4.576629485471,14.5));
#17150=CARTESIAN_POINT('Origin',(-20.1,6.475,12.5));
#17151=CARTESIAN_POINT('',(-15.87105808376,6.475,12.5));
#17152=CARTESIAN_POINT('',(-20.1,6.475,12.5));
#17153=CARTESIAN_POINT('',(-15.87105808376,6.475,14.5));
#17154=CARTESIAN_POINT('',(-15.87105808376,6.475,12.5));
#17155=CARTESIAN_POINT('',(-20.1,6.475,14.5));
#17156=CARTESIAN_POINT('Origin',(0.,0.,12.5));
#17157=CARTESIAN_POINT('',(0.,7.975,12.5));
#17158=CARTESIAN_POINT('',(-15.87105808376,6.475,12.5));
#17159=CARTESIAN_POINT('Origin',(-14.5,7.975,12.5));
#17160=CARTESIAN_POINT('Origin',(-15.,-48.1,14.5));
#17161=CARTESIAN_POINT('',(-13.475,-48.1,12.5));
#17162=CARTESIAN_POINT('',(-15.,-48.1,12.5));
#17163=CARTESIAN_POINT('',(-13.475,-48.1,12.5));
#17164=CARTESIAN_POINT('',(-15.,-48.1,14.5));
#17165=CARTESIAN_POINT('Origin',(0.,0.,12.5));
#17166=CARTESIAN_POINT('',(-13.475,-43.87105808376,12.5));
#17167=CARTESIAN_POINT('',(-11.1002577388094,-42.5000000000011,12.5));
#17168=CARTESIAN_POINT('',(-13.475,-43.87105808376,12.5));
#17169=CARTESIAN_POINT('',(-13.475,0.,12.5));
#17170=CARTESIAN_POINT('',(-12.5,-42.5,12.5));
#17171=CARTESIAN_POINT('Origin',(-12.5,-40.5,12.5));
#17172=CARTESIAN_POINT('',(-14.5,-42.5,12.5));
#17173=CARTESIAN_POINT('Origin',(-12.5,-40.5,20.63971317669));
#17174=CARTESIAN_POINT('',(-12.5,-42.5,-12.5));
#17175=CARTESIAN_POINT('',(-12.5,-42.5,20.63971317669));
#17176=CARTESIAN_POINT('Origin',(-12.5,-40.5,-12.5));
#17177=CARTESIAN_POINT('Origin',(0.,0.,-12.5));
#17178=CARTESIAN_POINT('',(-11.1002577388094,-42.5000000000011,-12.5));
#17179=CARTESIAN_POINT('',(0.,-42.5,-12.5));
#17180=CARTESIAN_POINT('',(-13.475,-48.1,-12.5));
#17181=CARTESIAN_POINT('',(0.,-48.1,-12.5));
#17182=CARTESIAN_POINT('',(-13.475,-43.87105808376,-12.5));
#17183=CARTESIAN_POINT('',(-13.475,0.,-12.5));
#17184=CARTESIAN_POINT('',(-13.475,-43.87105808376,-12.5));
#17185=CARTESIAN_POINT('Origin',(-15.,-48.1,-14.5));
#17186=CARTESIAN_POINT('',(-13.475,-48.1,-12.5));
#17187=CARTESIAN_POINT('',(0.,-48.1,-14.5));
#17188=CARTESIAN_POINT('Origin',(0.,0.,-14.5));
#17189=CARTESIAN_POINT('Origin',(0.,0.,-14.5));
#17190=CARTESIAN_POINT('',(-19.1,-39.25,-14.5));
#17191=CARTESIAN_POINT('',(0.,-39.25,-14.5));
#17192=CARTESIAN_POINT('',(-19.1,-21.975,-14.5));
#17193=CARTESIAN_POINT('',(-19.1,0.,-14.5));
#17194=CARTESIAN_POINT('',(0.,-21.975,-14.5));
#17195=CARTESIAN_POINT('Origin',(-13.75,-39.25,-5.));
#17196=CARTESIAN_POINT('',(-19.1,-39.25,-5.));
#17197=CARTESIAN_POINT('',(-19.1,-39.25,-5.));
#17198=CARTESIAN_POINT('',(-13.75,-39.25,-5.));
#17199=CARTESIAN_POINT('Origin',(-14.5,-38.525,12.5));
#17200=CARTESIAN_POINT('',(-13.75,-38.525,12.5));
#17201=CARTESIAN_POINT('',(-14.5,-38.525,12.5));
#17202=CARTESIAN_POINT('',(-13.75,-38.525,-5.));
#17203=CARTESIAN_POINT('',(-13.75,-38.525,12.5));
#17204=CARTESIAN_POINT('',(-14.5,-38.525,-5.));
#17205=CARTESIAN_POINT('Origin',(0.,0.,12.5));
#17206=CARTESIAN_POINT('',(-13.75,-22.475,12.5));
#17207=CARTESIAN_POINT('',(0.,-22.475,12.5));
#17208=CARTESIAN_POINT('',(-13.75,0.,12.5));
#17209=CARTESIAN_POINT('Origin',(-13.75,-22.475,12.5));
#17210=CARTESIAN_POINT('',(-13.75,-22.475,-5.));
#17211=CARTESIAN_POINT('',(-13.75,-22.475,12.5));
#17212=CARTESIAN_POINT('',(-13.75,-22.475,-5.));
#17213=CARTESIAN_POINT('Origin',(-19.1,-21.75,-5.));
#17214=CARTESIAN_POINT('',(-19.1,-21.75,-12.5));
#17215=CARTESIAN_POINT('',(-19.1,-21.75,-5.));
#17216=CARTESIAN_POINT('',(-19.1,-21.75,-5.));
#17217=CARTESIAN_POINT('',(-19.1,-21.75,-5.));
#17218=CARTESIAN_POINT('',(-19.1,-21.75,-12.5));
#17219=CARTESIAN_POINT('Origin',(0.,0.,-12.5));
#17220=CARTESIAN_POINT('',(-19.1,-21.975,-12.5));
#17221=CARTESIAN_POINT('',(0.,-21.975,-12.5));
#17222=CARTESIAN_POINT('',(-19.1,0.,-12.5));
#17223=CARTESIAN_POINT('',(-15.87105808376,-20.475,-12.5));
#17224=CARTESIAN_POINT('',(-14.5,-18.10025773881,-12.5));
#17225=CARTESIAN_POINT('',(0.,-20.475,-12.5));
#17226=CARTESIAN_POINT('Origin',(0.,0.,-12.5));
#17227=CARTESIAN_POINT('',(-14.4421161675114,-18.0000000000008,-12.5));
#17228=CARTESIAN_POINT('',(-15.87105808376,-15.525,-12.5));
#17229=CARTESIAN_POINT('',(-14.44211616751,-18.,-12.5));
#17230=CARTESIAN_POINT('Origin',(0.,0.,-12.5));
#17231=CARTESIAN_POINT('',(0.,-14.025,-12.5));
#17232=CARTESIAN_POINT('',(-15.87105808376,-15.525,-12.5));
#17233=CARTESIAN_POINT('',(0.,-15.525,-12.5));
#17234=CARTESIAN_POINT('',(-15.87105808376,-15.525,-12.5));
#17235=CARTESIAN_POINT('Origin',(-14.5,-14.025,-12.5));
#17236=CARTESIAN_POINT('',(-14.5,-14.025,-14.5));
#17237=CARTESIAN_POINT('Origin',(0.,0.,-14.5));
#17238=CARTESIAN_POINT('',(0.,0.025,-14.5));
#17239=CARTESIAN_POINT('Origin',(-20.1,0.025,-12.5));
#17240=CARTESIAN_POINT('',(-20.1,0.025,-12.5));
#17241=CARTESIAN_POINT('Origin',(0.,0.,-12.5));
#17242=CARTESIAN_POINT('',(-15.87105808376,1.525,-12.5));
#17243=CARTESIAN_POINT('',(-14.5,3.899742261193,-12.5));
#17244=CARTESIAN_POINT('',(0.,1.525,-12.5));
#17245=CARTESIAN_POINT('Origin',(0.,0.,-12.5));
#17246=CARTESIAN_POINT('',(-14.4421161675114,3.99999999999919,-12.5));
#17247=CARTESIAN_POINT('',(-15.87105808376,6.475,-12.5));
#17248=CARTESIAN_POINT('',(-14.44211616751,4.,-12.5));
#17249=CARTESIAN_POINT('Origin',(0.,0.,-12.5));
#17250=CARTESIAN_POINT('',(0.,7.975,-12.5));
#17251=CARTESIAN_POINT('',(-15.87105808376,6.475,-12.5));
#17252=CARTESIAN_POINT('',(0.,6.475,-12.5));
#17253=CARTESIAN_POINT('',(-15.87105808376,6.475,-12.5));
#17254=CARTESIAN_POINT('Origin',(-14.5,7.975,-12.5));
#17255=CARTESIAN_POINT('Origin',(0.,0.,12.5));
#17256=CARTESIAN_POINT('',(-14.4421161675114,3.99999999999919,12.5));
#17257=CARTESIAN_POINT('',(-14.44211616751,4.,12.5));
#17258=CARTESIAN_POINT('',(-14.5,4.100257738807,12.5));
#17259=CARTESIAN_POINT('Origin',(0.,0.,12.5));
#17260=CARTESIAN_POINT('',(0.,0.025,12.5));
#17261=CARTESIAN_POINT('',(-15.87105808376,1.525,12.5));
#17262=CARTESIAN_POINT('',(0.,1.525,12.5));
#17263=CARTESIAN_POINT('',(-14.5,3.899742261193,12.5));
#17264=CARTESIAN_POINT('Origin',(-20.1,0.025,12.5));
#17265=CARTESIAN_POINT('',(-20.1,0.025,14.5));
#17266=CARTESIAN_POINT('Origin',(0.,0.,14.5));
#17267=CARTESIAN_POINT('',(0.,-14.025,14.5));
#17268=CARTESIAN_POINT('Origin',(-14.5,-14.025,12.5));
#17269=CARTESIAN_POINT('',(-14.5,-14.025,12.5));
#17270=CARTESIAN_POINT('Origin',(0.,0.,12.5));
#17271=CARTESIAN_POINT('',(-15.87105808376,-15.525,12.5));
#17272=CARTESIAN_POINT('',(-15.87105808376,-15.525,12.5));
#17273=CARTESIAN_POINT('',(0.,-15.525,12.5));
#17274=CARTESIAN_POINT('Origin',(0.,0.,12.5));
#17275=CARTESIAN_POINT('',(-14.4421161675114,-18.0000000000008,12.5));
#17276=CARTESIAN_POINT('',(-14.44211616751,-18.,12.5));
#17277=CARTESIAN_POINT('',(-14.5,-17.89974226119,12.5));
#17278=CARTESIAN_POINT('Origin',(0.,0.,12.5));
#17279=CARTESIAN_POINT('',(0.,-21.975,12.5));
#17280=CARTESIAN_POINT('',(-15.87105808376,-20.475,12.5));
#17281=CARTESIAN_POINT('',(0.,-20.475,12.5));
#17282=CARTESIAN_POINT('',(-14.5,-18.10025773881,12.5));
#17283=CARTESIAN_POINT('Origin',(-20.1,-21.975,12.5));
#17284=CARTESIAN_POINT('',(-20.1,-21.975,14.5));
#17285=CARTESIAN_POINT('Origin',(0.,0.,14.5));
#17286=CARTESIAN_POINT('Origin',(0.,0.,14.5));
#17287=CARTESIAN_POINT('Origin',(-20.1,6.475,-12.5));
#17288=CARTESIAN_POINT('',(-15.87105808376,6.475,-14.5));
#17289=CARTESIAN_POINT('',(-15.87105808376,6.475,-12.5));
#17290=CARTESIAN_POINT('',(-20.1,6.475,-14.5));
#17291=CARTESIAN_POINT('Origin',(0.,0.,-14.5));
#17292=CARTESIAN_POINT('',(13.475,-43.87105808376,-14.5));
#17293=CARTESIAN_POINT('',(13.475,-43.87105808376,-14.5));
#17294=CARTESIAN_POINT('',(11.,-42.44211616751,-14.5));
#17295=CARTESIAN_POINT('',(11.,-42.44211616751,-14.5));
#17296=CARTESIAN_POINT('',(8.525,-43.87105808376,-14.5));
#17297=CARTESIAN_POINT('',(8.525,-43.87105808376,-14.5));
#17298=CARTESIAN_POINT('',(8.525,0.,-14.5));
#17299=CARTESIAN_POINT('Origin',(0.,0.,-14.5));
#17300=CARTESIAN_POINT('',(15.8710580837579,-15.5249999999988,-14.5));
#17301=CARTESIAN_POINT('',(0.,-15.525,-14.5));
#17302=CARTESIAN_POINT('',(14.44211616751,-18.,-14.5));
#17303=CARTESIAN_POINT('',(14.44211616751,-18.,-14.5));
#17304=CARTESIAN_POINT('',(15.87105808376,-20.475,-14.5));
#17305=CARTESIAN_POINT('',(15.87105808376,-20.475,-14.5));
#17306=CARTESIAN_POINT('',(0.,-20.475,-14.5));
#17307=CARTESIAN_POINT('Origin',(0.,0.,-14.5));
#17308=CARTESIAN_POINT('',(15.87105808376,6.475,-14.5));
#17309=CARTESIAN_POINT('',(0.,6.475,-14.5));
#17310=CARTESIAN_POINT('',(14.44211616751,4.,-14.5));
#17311=CARTESIAN_POINT('',(14.44211616751,4.,-14.5));
#17312=CARTESIAN_POINT('',(15.87105808376,1.525,-14.5));
#17313=CARTESIAN_POINT('',(15.87105808376,1.525,-14.5));
#17314=CARTESIAN_POINT('',(0.,1.525,-14.5));
#17315=CARTESIAN_POINT('Origin',(0.,0.,-14.5));
#17316=CARTESIAN_POINT('',(-8.52499999999879,-43.8710580837579,-14.5));
#17317=CARTESIAN_POINT('',(-8.525,0.,-14.5));
#17318=CARTESIAN_POINT('',(-10.9999999999988,-42.4421161675121,-14.5));
#17319=CARTESIAN_POINT('',(-11.,-42.44211616751,-14.5));
#17320=CARTESIAN_POINT('',(-13.475,-43.87105808376,-14.5));
#17321=CARTESIAN_POINT('',(-13.475,-43.87105808376,-14.5));
#17322=CARTESIAN_POINT('',(-13.475,-48.1,-14.5));
#17323=CARTESIAN_POINT('Origin',(0.,0.,-14.5));
#17324=CARTESIAN_POINT('',(-15.87105808376,-20.475,-14.5));
#17325=CARTESIAN_POINT('',(0.,-20.475,-14.5));
#17326=CARTESIAN_POINT('',(-14.44211616751,-18.,-14.5));
#17327=CARTESIAN_POINT('',(-14.44211616751,-18.,-14.5));
#17328=CARTESIAN_POINT('',(-15.87105808376,-15.525,-14.5));
#17329=CARTESIAN_POINT('',(-15.87105808376,-15.525,-14.5));
#17330=CARTESIAN_POINT('',(0.,-15.525,-14.5));
#17331=CARTESIAN_POINT('Origin',(0.,0.,-14.5));
#17332=CARTESIAN_POINT('',(-15.87105808376,1.525,-14.5));
#17333=CARTESIAN_POINT('',(0.,1.525,-14.5));
#17334=CARTESIAN_POINT('',(-14.44211616751,4.,-14.5));
#17335=CARTESIAN_POINT('',(-14.44211616751,4.,-14.5));
#17336=CARTESIAN_POINT('',(-15.87105808376,6.475,-14.5));
#17337=CARTESIAN_POINT('Origin',(20.1,1.525,-12.5));
#17338=CARTESIAN_POINT('',(15.87105808376,1.525,-12.5));
#17339=CARTESIAN_POINT('',(15.87105808376,1.525,-12.5));
#17340=CARTESIAN_POINT('',(20.1,1.525,-12.5));
#17341=CARTESIAN_POINT('Origin',(14.5,0.025,-12.5));
#17342=CARTESIAN_POINT('',(14.5,0.025,-14.5));
#17343=CARTESIAN_POINT('',(14.5,0.025,-12.5));
#17344=CARTESIAN_POINT('Origin',(0.,0.,-14.5));
#17345=CARTESIAN_POINT('',(0.,-14.025,-14.5));
#17346=CARTESIAN_POINT('Origin',(20.1,-14.025,-12.5));
#17347=CARTESIAN_POINT('',(20.1,-14.025,-12.5));
#17348=CARTESIAN_POINT('Origin',(15.87105808376,-15.525,-12.5));
#17349=CARTESIAN_POINT('',(15.8710580837595,-15.525,-12.5));
#17350=CARTESIAN_POINT('',(15.87105808376,-15.525,-12.5));
#17351=CARTESIAN_POINT('',(15.87105808376,-15.525,-12.5));
#17352=CARTESIAN_POINT('Origin',(20.1,-20.475,-12.5));
#17353=CARTESIAN_POINT('',(15.87105808376,-20.475,-12.5));
#17354=CARTESIAN_POINT('',(15.87105808376,-20.475,-12.5));
#17355=CARTESIAN_POINT('',(20.1,-20.475,-12.5));
#17356=CARTESIAN_POINT('Origin',(14.5,-21.975,-12.5));
#17357=CARTESIAN_POINT('',(19.1,-21.975,-14.5));
#17358=CARTESIAN_POINT('',(14.5,-21.975,-14.5));
#17359=CARTESIAN_POINT('',(19.1,-21.975,-12.5));
#17360=CARTESIAN_POINT('',(14.5,-21.975,-12.5));
#17361=CARTESIAN_POINT('',(19.1,-21.975,-12.5));
#17362=CARTESIAN_POINT('Origin',(0.,0.,-14.5));
#17363=CARTESIAN_POINT('',(19.1,-39.25,-14.5));
#17364=CARTESIAN_POINT('',(19.1,0.,-14.5));
#17365=CARTESIAN_POINT('',(0.,-39.25,-14.5));
#17366=CARTESIAN_POINT('Origin',(0.,0.,-14.5));
#17367=CARTESIAN_POINT('',(-15.,-48.1,-14.5));
#17368=CARTESIAN_POINT('Origin',(8.525,-48.1,-12.5));
#17369=CARTESIAN_POINT('',(8.525,-43.87105808376,-12.5));
#17370=CARTESIAN_POINT('',(8.525,-43.87105808376,-12.5));
#17371=CARTESIAN_POINT('',(8.525,-48.1,-12.5));
#17372=CARTESIAN_POINT('Origin',(7.025,-42.5,-12.5));
#17373=CARTESIAN_POINT('',(7.025,-42.5,-14.5));
#17374=CARTESIAN_POINT('',(7.025,-42.5,-14.5));
#17375=CARTESIAN_POINT('',(7.025,-42.5,-12.5));
#17376=CARTESIAN_POINT('',(7.025,-42.5,-12.5));
#17377=CARTESIAN_POINT('',(7.025,-42.5,-12.5));
#17378=CARTESIAN_POINT('Origin',(0.,0.,-14.5));
#17379=CARTESIAN_POINT('',(-7.025,-42.5,-14.5));
#17380=CARTESIAN_POINT('',(-7.025,0.,-14.5));
#17381=CARTESIAN_POINT('',(0.,-42.5,-14.5));
#17382=CARTESIAN_POINT('Origin',(-7.025,-48.1,-12.5));
#17383=CARTESIAN_POINT('',(-7.025,-42.5,-12.5));
#17384=CARTESIAN_POINT('',(-7.025,-48.1,-12.5));
#17385=CARTESIAN_POINT('',(-7.025,-42.5,-12.5));
#17386=CARTESIAN_POINT('Origin',(-8.525,-43.87105808376,-12.5));
#17387=CARTESIAN_POINT('',(-8.52499999999757,-43.8710580837558,-12.5));
#17388=CARTESIAN_POINT('',(-8.525,-43.87105808376,-12.5));
#17389=CARTESIAN_POINT('',(-8.525,-43.87105808376,-12.5));
#17390=CARTESIAN_POINT('Origin',(-20.1,-21.975,-12.5));
#17391=CARTESIAN_POINT('',(-19.1,-21.975,-12.5));
#17392=CARTESIAN_POINT('Origin',(-15.87105808376,-20.475,-12.5));
#17393=CARTESIAN_POINT('',(-15.87105808376,-20.475,-12.5));
#17394=CARTESIAN_POINT('Origin',(-20.1,-15.525,-12.5));
#17395=CARTESIAN_POINT('',(-15.87105808376,-15.525,-12.5));
#17396=CARTESIAN_POINT('Origin',(-15.87105808376,1.525,-12.5));
#17397=CARTESIAN_POINT('',(-15.87105808376,1.525,-12.5));
#17398=CARTESIAN_POINT('Origin',(-6.65,8.804969405268,-19.));
#17399=CARTESIAN_POINT('Origin',(-6.65,9.000000000629,-19.));
#17400=CARTESIAN_POINT('Origin',(-10.5,9.00000000000002,-19.));
#17401=CARTESIAN_POINT('Origin',(-10.5,5.15,-19.));
#17402=CARTESIAN_POINT('Origin',(-14.67485779376,5.15,-19.));
#17403=CARTESIAN_POINT('Origin',(-13.,5.15,-19.));
#17404=CARTESIAN_POINT('Origin',(-13.,-42.63464535978,-19.));
#17405=CARTESIAN_POINT('Origin',(-13.,5.15,-19.));
#17406=CARTESIAN_POINT('Origin',(-13.,-34.65,-19.));
#17407=CARTESIAN_POINT('Origin',(14.65914844686,-34.65,-19.));
#17408=CARTESIAN_POINT('Origin',(-10.5,-34.65,-19.));
#17409=CARTESIAN_POINT('Origin',(-13.,-34.65,-19.));
#17410=CARTESIAN_POINT('Origin',(-10.5000000000001,-38.5000000000001,-19.0000000000001));
#17411=CARTESIAN_POINT('Origin',(-6.65,-38.50000000054,-19.));
#17412=CARTESIAN_POINT('Origin',(-6.65,-42.69230397724,-19.));
#17413=CARTESIAN_POINT('Origin',(-6.65,-41.,-19.));
#17414=CARTESIAN_POINT('Origin',(13.69503059473,-41.,-19.));
#17415=CARTESIAN_POINT('Origin',(-6.65,-41.,-19.));
#17416=CARTESIAN_POINT('Origin',(6.65,-41.,-19.));
#17417=CARTESIAN_POINT('Origin',(6.65,9.717758793986,-19.));
#17418=CARTESIAN_POINT('Origin',(6.65,-38.5,-19.));
#17419=CARTESIAN_POINT('Origin',(6.65,-41.,-19.));
#17420=CARTESIAN_POINT('Origin',(10.5,-38.5,-19.));
#17421=CARTESIAN_POINT('Origin',(10.50000000054,-34.65,-19.));
#17422=CARTESIAN_POINT('Origin',(14.65914844686,-34.65,-19.));
#17423=CARTESIAN_POINT('Origin',(13.,-34.65,-19.));
#17424=CARTESIAN_POINT('Origin',(13.,9.639713176691,-19.));
#17425=CARTESIAN_POINT('Origin',(13.,-34.65,-19.));
#17426=CARTESIAN_POINT('Origin',(13.,5.15,-19.));
#17427=CARTESIAN_POINT('Origin',(-14.67485779376,5.15,-19.));
#17428=CARTESIAN_POINT('Origin',(10.5,5.15,-19.));
#17429=CARTESIAN_POINT('Origin',(13.,5.15,-19.));
#17430=CARTESIAN_POINT('Origin',(10.5,8.99999999999997,-19.));
#17431=CARTESIAN_POINT('Origin',(6.65,9.,-19.));
#17432=CARTESIAN_POINT('Origin',(6.65,9.639713176691,-19.));
#17433=CARTESIAN_POINT('Origin',(18.417,7.975,-12.5));
#17434=CARTESIAN_POINT('',(18.417,7.975,-12.5));
#17435=CARTESIAN_POINT('Origin',(0.,0.,-12.5));
#17436=CARTESIAN_POINT('',(15.87105808376,6.475,-12.5));
#17437=CARTESIAN_POINT('',(14.5,4.100257738807,-12.5));
#17438=CARTESIAN_POINT('',(0.,6.475,-12.5));
#17439=CARTESIAN_POINT('Origin',(15.87105808376,6.475,-12.5));
#17440=CARTESIAN_POINT('',(15.87105808376,6.475,-12.5));
#17441=CARTESIAN_POINT('Origin',(18.417,7.975,12.5));
#17442=CARTESIAN_POINT('',(18.417,7.975,12.5));
#17443=CARTESIAN_POINT('Origin',(0.,0.,14.5));
#17444=CARTESIAN_POINT('',(0.,-21.975,14.5));
#17445=CARTESIAN_POINT('Origin',(14.5,-21.975,12.5));
#17446=CARTESIAN_POINT('',(14.5,-21.975,12.5));
#17447=CARTESIAN_POINT('Origin',(0.,0.,12.5));
#17448=CARTESIAN_POINT('',(15.87105808376,-20.475,12.5));
#17449=CARTESIAN_POINT('',(15.87105808376,-20.475,12.5));
#17450=CARTESIAN_POINT('',(0.,-20.475,12.5));
#17451=CARTESIAN_POINT('Origin',(0.,0.,12.5));
#17452=CARTESIAN_POINT('',(14.4421161675114,-17.9999999999992,12.5));
#17453=CARTESIAN_POINT('',(14.44211616751,-18.,12.5));
#17454=CARTESIAN_POINT('',(14.5,-18.10025773881,12.5));
#17455=CARTESIAN_POINT('Origin',(0.,0.,12.5));
#17456=CARTESIAN_POINT('',(0.,-14.025,12.5));
#17457=CARTESIAN_POINT('',(15.87105808376,-15.525,12.5));
#17458=CARTESIAN_POINT('',(0.,-15.525,12.5));
#17459=CARTESIAN_POINT('',(14.5,-17.89974226119,12.5));
#17460=CARTESIAN_POINT('Origin',(20.1,-14.025,12.5));
#17461=CARTESIAN_POINT('',(20.1,-14.025,14.5));
#17462=CARTESIAN_POINT('Origin',(0.,0.,14.5));
#17463=CARTESIAN_POINT('',(0.,0.025,14.5));
#17464=CARTESIAN_POINT('Origin',(14.5,0.025,12.5));
#17465=CARTESIAN_POINT('',(14.5,0.025,12.5));
#17466=CARTESIAN_POINT('Origin',(0.,0.,12.5));
#17467=CARTESIAN_POINT('',(15.87105808376,1.525,12.5));
#17468=CARTESIAN_POINT('',(15.87105808376,1.525,12.5));
#17469=CARTESIAN_POINT('',(0.,1.525,12.5));
#17470=CARTESIAN_POINT('Origin',(0.,0.,12.5));
#17471=CARTESIAN_POINT('',(14.4421161675114,4.00000000000081,12.5));
#17472=CARTESIAN_POINT('',(14.44211616751,4.,12.5));
#17473=CARTESIAN_POINT('',(14.5,3.899742261193,12.5));
#17474=CARTESIAN_POINT('Origin',(0.,0.,12.5));
#17475=CARTESIAN_POINT('',(15.87105808376,6.475,12.5));
#17476=CARTESIAN_POINT('',(0.,6.475,12.5));
#17477=CARTESIAN_POINT('',(14.5,4.100257738807,12.5));
#17478=CARTESIAN_POINT('Origin',(0.,0.,-12.5));
#17479=CARTESIAN_POINT('',(14.44211616751,4.,-12.5));
#17480=CARTESIAN_POINT('',(14.5,3.899742261193,-12.5));
#17481=CARTESIAN_POINT('',(14.44211616751,4.,-12.5));
#17482=CARTESIAN_POINT('Origin',(0.,0.,-12.5));
#17483=CARTESIAN_POINT('',(15.87105808376,1.525,-12.5));
#17484=CARTESIAN_POINT('Origin',(0.,0.,-12.5));
#17485=CARTESIAN_POINT('',(14.5,-17.89974226119,-12.5));
#17486=CARTESIAN_POINT('Origin',(0.,0.,-12.5));
#17487=CARTESIAN_POINT('',(14.44211616751,-18.,-12.5));
#17488=CARTESIAN_POINT('',(14.5,-18.10025773881,-12.5));
#17489=CARTESIAN_POINT('',(14.44211616751,-18.,-12.5));
#17490=CARTESIAN_POINT('Origin',(0.,0.,-12.5));
#17491=CARTESIAN_POINT('',(15.87105808376,-20.475,-12.5));
#17492=CARTESIAN_POINT('',(19.1,-21.75,-12.5));
#17493=CARTESIAN_POINT('',(0.,-21.75,-12.5));
#17494=CARTESIAN_POINT('',(19.1,0.,-12.5));
#17495=CARTESIAN_POINT('Origin',(13.75,-21.75,-5.));
#17496=CARTESIAN_POINT('',(19.1,-21.75,-5.));
#17497=CARTESIAN_POINT('',(19.1,-21.75,-5.));
#17498=CARTESIAN_POINT('',(13.75,-21.75,-5.));
#17499=CARTESIAN_POINT('Origin',(14.5,-22.475,12.5));
#17500=CARTESIAN_POINT('',(13.75,-22.475,12.5));
#17501=CARTESIAN_POINT('',(14.5,-22.475,12.5));
#17502=CARTESIAN_POINT('',(13.75,-22.475,-5.));
#17503=CARTESIAN_POINT('',(13.75,-22.475,12.5));
#17504=CARTESIAN_POINT('',(14.5,-22.475,-5.));
#17505=CARTESIAN_POINT('Origin',(0.,0.,12.5));
#17506=CARTESIAN_POINT('',(13.75,-38.525,12.5));
#17507=CARTESIAN_POINT('',(0.,-38.525,12.5));
#17508=CARTESIAN_POINT('',(13.75,0.,12.5));
#17509=CARTESIAN_POINT('Origin',(13.75,-38.525,12.5));
#17510=CARTESIAN_POINT('',(13.75,-38.525,-5.));
#17511=CARTESIAN_POINT('',(13.75,-38.525,12.5));
#17512=CARTESIAN_POINT('',(13.75,-38.525,-5.));
#17513=CARTESIAN_POINT('Origin',(19.1,-39.25,-5.));
#17514=CARTESIAN_POINT('',(19.1,-39.25,-5.));
#17515=CARTESIAN_POINT('',(19.1,-39.25,-5.));
#17516=CARTESIAN_POINT('',(19.1,-39.25,-5.));
#17517=CARTESIAN_POINT('Origin',(-15.,-48.1,-14.5));
#17518=CARTESIAN_POINT('',(13.475,-48.1,-12.5));
#17519=CARTESIAN_POINT('',(-15.,-48.1,-12.5));
#17520=CARTESIAN_POINT('',(13.475,-48.1,-12.5));
#17521=CARTESIAN_POINT('Origin',(0.,0.,-12.5));
#17522=CARTESIAN_POINT('',(12.5,-42.5,-12.5));
#17523=CARTESIAN_POINT('Origin',(12.5,-40.5,-12.5));
#17524=CARTESIAN_POINT('',(11.10025773881,-42.5000000000001,-12.5));
#17525=CARTESIAN_POINT('',(0.,-42.5,-12.5));
#17526=CARTESIAN_POINT('',(13.475,-43.87105808376,-12.5));
#17527=CARTESIAN_POINT('',(11.10025773881,-42.5,-12.5));
#17528=CARTESIAN_POINT('',(13.475,0.,-12.5));
#17529=CARTESIAN_POINT('Origin',(12.5,-40.5,20.63971317669));
#17530=CARTESIAN_POINT('',(12.5,-42.5,12.5));
#17531=CARTESIAN_POINT('Origin',(12.5,-40.5,12.5));
#17532=CARTESIAN_POINT('',(12.5,-42.5,20.63971317669));
#17533=CARTESIAN_POINT('Origin',(0.,0.,12.5));
#17534=CARTESIAN_POINT('',(13.475,-48.1,12.5));
#17535=CARTESIAN_POINT('',(0.,-48.1,12.5));
#17536=CARTESIAN_POINT('',(13.475,-43.87105808376,12.5));
#17537=CARTESIAN_POINT('',(13.475,0.,12.5));
#17538=CARTESIAN_POINT('',(11.10025773881,-42.5000000000001,12.5));
#17539=CARTESIAN_POINT('',(11.10025773881,-42.5,12.5));
#17540=CARTESIAN_POINT('',(0.,-42.5,12.5));
#17541=CARTESIAN_POINT('Origin',(-15.,-48.1,14.5));
#17542=CARTESIAN_POINT('',(-15.,-48.1,14.5));
#17543=CARTESIAN_POINT('',(13.475,-48.1,12.5));
#17544=CARTESIAN_POINT('Origin',(0.,0.,14.5));
#17545=CARTESIAN_POINT('Origin',(15.87105808376,6.475,12.5));
#17546=CARTESIAN_POINT('',(15.87105808376,6.475,14.5));
#17547=CARTESIAN_POINT('',(15.87105808376,6.475,14.5));
#17548=CARTESIAN_POINT('',(15.87105808376,6.475,12.5));
#17549=CARTESIAN_POINT('Origin',(0.,0.,14.5));
#17550=CARTESIAN_POINT('',(13.475,-43.87105808376,14.5));
#17551=CARTESIAN_POINT('',(13.475,0.,14.5));
#17552=CARTESIAN_POINT('',(8.525,-43.87105808376,14.5));
#17553=CARTESIAN_POINT('',(8.525,0.,14.5));
#17554=CARTESIAN_POINT('',(11.,-42.44211616751,14.5));
#17555=CARTESIAN_POINT('',(8.525,-43.87105808376,14.5));
#17556=CARTESIAN_POINT('',(11.,-42.44211616751,14.5));
#17557=CARTESIAN_POINT('Origin',(0.,0.,14.5));
#17558=CARTESIAN_POINT('',(14.4421161675114,-17.9999999999992,14.5));
#17559=CARTESIAN_POINT('',(15.87105808376,-15.525,14.5));
#17560=CARTESIAN_POINT('',(14.44211616751,-18.,14.5));
#17561=CARTESIAN_POINT('',(0.,-15.525,14.5));
#17562=CARTESIAN_POINT('',(15.87105808376,-20.475,14.5));
#17563=CARTESIAN_POINT('',(0.,-20.475,14.5));
#17564=CARTESIAN_POINT('',(15.87105808376,-20.475,14.5));
#17565=CARTESIAN_POINT('Origin',(0.,0.,14.5));
#17566=CARTESIAN_POINT('',(15.87105808376,1.525,14.5));
#17567=CARTESIAN_POINT('',(0.,1.525,14.5));
#17568=CARTESIAN_POINT('',(14.4421161675114,4.00000000000081,14.5));
#17569=CARTESIAN_POINT('',(15.87105808376,1.525,14.5));
#17570=CARTESIAN_POINT('',(14.44211616751,4.,14.5));
#17571=CARTESIAN_POINT('Origin',(0.,0.,14.5));
#17572=CARTESIAN_POINT('',(-8.52499999999879,-43.8710580837579,14.5));
#17573=CARTESIAN_POINT('',(-8.525,0.,14.5));
#17574=CARTESIAN_POINT('',(-13.475,-43.87105808376,14.5));
#17575=CARTESIAN_POINT('',(-13.475,0.,14.5));
#17576=CARTESIAN_POINT('',(-10.9999999999988,-42.4421161675121,14.5));
#17577=CARTESIAN_POINT('',(-13.475,-43.87105808376,14.5));
#17578=CARTESIAN_POINT('',(-11.,-42.44211616751,14.5));
#17579=CARTESIAN_POINT('Origin',(0.,0.,14.5));
#17580=CARTESIAN_POINT('',(-14.4421161675114,-18.0000000000008,14.5));
#17581=CARTESIAN_POINT('',(-15.87105808376,-20.475,14.5));
#17582=CARTESIAN_POINT('',(-14.44211616751,-18.,14.5));
#17583=CARTESIAN_POINT('',(0.,-20.475,14.5));
#17584=CARTESIAN_POINT('',(-15.87105808376,-15.525,14.5));
#17585=CARTESIAN_POINT('',(0.,-15.525,14.5));
#17586=CARTESIAN_POINT('',(-15.87105808376,-15.525,14.5));
#17587=CARTESIAN_POINT('Origin',(0.,0.,14.5));
#17588=CARTESIAN_POINT('',(-15.87105808376,1.525,14.5));
#17589=CARTESIAN_POINT('',(0.,1.525,14.5));
#17590=CARTESIAN_POINT('',(-14.4421161675114,3.99999999999919,14.5));
#17591=CARTESIAN_POINT('',(-15.87105808376,6.475,14.5));
#17592=CARTESIAN_POINT('',(-14.44211616751,4.,14.5));
#17593=CARTESIAN_POINT('Origin',(20.1,1.525,12.5));
#17594=CARTESIAN_POINT('',(15.87105808376,1.525,12.5));
#17595=CARTESIAN_POINT('Origin',(15.87105808376,-15.525,12.5));
#17596=CARTESIAN_POINT('',(15.87105808376,-15.525,12.5));
#17597=CARTESIAN_POINT('Origin',(20.1,-20.475,12.5));
#17598=CARTESIAN_POINT('',(15.87105808376,-20.475,12.5));
#17599=CARTESIAN_POINT('Origin',(8.525,-48.1,12.5));
#17600=CARTESIAN_POINT('',(8.525,-43.87105808376,12.5));
#17601=CARTESIAN_POINT('',(8.525,-48.1,12.5));
#17602=CARTESIAN_POINT('',(8.525,-43.87105808376,12.5));
#17603=CARTESIAN_POINT('Origin',(7.025,-42.5,12.5));
#17604=CARTESIAN_POINT('',(7.025,-42.5,14.5));
#17605=CARTESIAN_POINT('',(7.025,-42.5,14.5));
#17606=CARTESIAN_POINT('',(7.025,-42.5,12.5));
#17607=CARTESIAN_POINT('',(7.025,-42.5,12.5));
#17608=CARTESIAN_POINT('',(7.025,-42.5,12.5));
#17609=CARTESIAN_POINT('Origin',(0.,0.,14.5));
#17610=CARTESIAN_POINT('',(-7.025,-42.5,14.5));
#17611=CARTESIAN_POINT('',(-7.025,0.,14.5));
#17612=CARTESIAN_POINT('',(0.,-42.5,14.5));
#17613=CARTESIAN_POINT('Origin',(-7.025,-48.1,12.5));
#17614=CARTESIAN_POINT('',(-7.025,-42.5,12.5));
#17615=CARTESIAN_POINT('',(-7.025,-48.1,12.5));
#17616=CARTESIAN_POINT('',(-7.025,-42.5,12.5));
#17617=CARTESIAN_POINT('Origin',(-8.525,-43.87105808376,12.5));
#17618=CARTESIAN_POINT('',(-8.52499999999757,-43.8710580837558,12.5));
#17619=CARTESIAN_POINT('',(-8.525,-43.87105808376,12.5));
#17620=CARTESIAN_POINT('',(-8.525,-43.87105808376,12.5));
#17621=CARTESIAN_POINT('Origin',(-15.87105808376,-20.475,12.5));
#17622=CARTESIAN_POINT('',(-15.87105808376,-20.475,12.5));
#17623=CARTESIAN_POINT('Origin',(-20.1,-15.525,12.5));
#17624=CARTESIAN_POINT('',(-15.87105808376,-15.525,12.5));
#17625=CARTESIAN_POINT('Origin',(-15.87105808376,1.525,12.5));
#17626=CARTESIAN_POINT('',(-15.87105808376,1.525,12.5));
#17627=CARTESIAN_POINT('Origin',(0.,0.,25.));
#17628=CARTESIAN_POINT('Origin',(-15.87105808376,6.475,12.5));
#17629=CARTESIAN_POINT('',(-14.4421161675142,3.99999999999757,12.5));
#17630=CARTESIAN_POINT('Origin',(-13.475,-48.1,12.5));
#17631=CARTESIAN_POINT('',(-13.475,-43.87105808376,12.5));
#17632=CARTESIAN_POINT('Origin',(-13.475,-43.87105808376,12.5));
#17633=CARTESIAN_POINT('',(-10.9999999999983,-42.4421161675124,12.5));
#17634=CARTESIAN_POINT('',(-13.475,-43.87105808376,12.5));
#17635=CARTESIAN_POINT('',(-10.9999999999976,-42.4421161675142,12.5));
#17636=CARTESIAN_POINT('Origin',(-14.5,-42.5,-20.5));
#17637=CARTESIAN_POINT('',(10.8997422611913,-42.5000000000022,-12.5));
#17638=CARTESIAN_POINT('',(-14.5,-42.5,-12.5));
#17639=CARTESIAN_POINT('',(10.8997422611913,-42.5000000000022,12.5));
#17640=CARTESIAN_POINT('',(-14.5,-42.5,12.5));
#17641=CARTESIAN_POINT('',(-14.5,-42.5,12.5));
#17642=CARTESIAN_POINT('',(-10.8997422611901,-42.5000000000001,12.5));
#17643=CARTESIAN_POINT('',(-14.5,-42.5,12.5));
#17644=CARTESIAN_POINT('',(-14.5,-42.5,12.5));
#17645=CARTESIAN_POINT('',(-10.8997422611901,-42.5000000000001,-12.5));
#17646=CARTESIAN_POINT('',(-14.5,-42.5,-12.5));
#17647=CARTESIAN_POINT('',(-14.5,-42.5,-12.5));
#17648=CARTESIAN_POINT('',(-14.5,-42.5,-12.5));
#17649=CARTESIAN_POINT('Origin',(-13.475,-43.87105808376,-12.5));
#17650=CARTESIAN_POINT('',(-10.9999999999984,-42.4421161675128,-12.5));
#17651=CARTESIAN_POINT('',(-10.9999999999976,-42.4421161675142,-12.5));
#17652=CARTESIAN_POINT('',(-13.475,-43.87105808376,-12.5));
#17653=CARTESIAN_POINT('',(-13.475,-43.87105808376,-12.5));
#17654=CARTESIAN_POINT('Origin',(-13.475,-48.1,-12.5));
#17655=CARTESIAN_POINT('Origin',(-19.1,-39.25,-5.));
#17656=CARTESIAN_POINT('',(-19.1,-39.25,-5.));
#17657=CARTESIAN_POINT('Origin',(0.,0.,-5.));
#17658=CARTESIAN_POINT('',(-13.75,0.,-5.));
#17659=CARTESIAN_POINT('',(-13.98,-37.95,-5.));
#17660=CARTESIAN_POINT('',(-13.98,-23.05,-5.));
#17661=CARTESIAN_POINT('',(-13.98,0.,-5.));
#17662=CARTESIAN_POINT('',(-18.88,-37.95,-5.));
#17663=CARTESIAN_POINT('',(0.,-37.95,-5.));
#17664=CARTESIAN_POINT('',(-18.88,-23.05,-5.));
#17665=CARTESIAN_POINT('',(-18.88,0.,-5.));
#17666=CARTESIAN_POINT('',(0.,-23.05,-5.));
#17667=CARTESIAN_POINT('Origin',(-13.75,-38.525,12.5));
#17668=CARTESIAN_POINT('Origin',(-14.44211616751,-18.,-12.5));
#17669=CARTESIAN_POINT('',(-14.44211616751,-18.,-12.5));
#17670=CARTESIAN_POINT('Origin',(-15.87105808376,-15.525,-12.5));
#17671=CARTESIAN_POINT('Origin',(-14.44211616751,4.,-12.5));
#17672=CARTESIAN_POINT('',(-14.44211616751,4.,-12.5));
#17673=CARTESIAN_POINT('Origin',(-15.87105808376,6.475,-12.5));
#17674=CARTESIAN_POINT('Origin',(-14.44211616751,4.,12.5));
#17675=CARTESIAN_POINT('Origin',(-15.87105808376,-15.525,12.5));
#17676=CARTESIAN_POINT('',(-14.4421161675142,-18.0000000000024,12.5));
#17677=CARTESIAN_POINT('Origin',(-14.44211616751,-18.,12.5));
#17678=CARTESIAN_POINT('Origin',(13.475,-43.87105808376,-12.5));
#17679=CARTESIAN_POINT('',(13.475,-43.87105808376,-12.5));
#17680=CARTESIAN_POINT('Origin',(11.,-42.44211616751,-12.5));
#17681=CARTESIAN_POINT('',(11.0000000000008,-42.4421161675114,-12.5));
#17682=CARTESIAN_POINT('',(11.,-42.44211616751,-12.5));
#17683=CARTESIAN_POINT('',(11.,-42.44211616751,-12.5));
#17684=CARTESIAN_POINT('Origin',(8.525,-43.87105808376,-12.5));
#17685=CARTESIAN_POINT('',(8.525,-43.87105808376,-12.5));
#17686=CARTESIAN_POINT('',(8.525,-43.87105808376,-12.5));
#17687=CARTESIAN_POINT('Origin',(14.44211616751,-18.,-12.5));
#17688=CARTESIAN_POINT('',(14.44211616751,-18.,-12.5));
#17689=CARTESIAN_POINT('Origin',(15.87105808376,-20.475,-12.5));
#17690=CARTESIAN_POINT('Origin',(14.44211616751,4.,-12.5));
#17691=CARTESIAN_POINT('',(14.44211616751,4.,-12.5));
#17692=CARTESIAN_POINT('Origin',(15.87105808376,1.525,-12.5));
#17693=CARTESIAN_POINT('Origin',(-11.,-42.44211616751,-12.5));
#17694=CARTESIAN_POINT('',(-11.,-42.44211616751,-12.5));
#17695=CARTESIAN_POINT('',(-11.,-42.44211616751,-12.5));
#17696=CARTESIAN_POINT('Origin',(19.1,-21.75,-5.));
#17697=CARTESIAN_POINT('',(19.1,-21.75,-5.));
#17698=CARTESIAN_POINT('Origin',(0.,0.,-12.5));
#17699=CARTESIAN_POINT('Origin',(0.,0.,-12.5));
#17700=CARTESIAN_POINT('Origin',(-13.,5.15,-19.));
#17701=CARTESIAN_POINT('Ctrl Pts',(-14.5000000000002,5.14999999999998,-18.9999999999996));
#17702=CARTESIAN_POINT('Ctrl Pts',(-14.5,5.1502683704716,-19.0070720743157));
#17703=CARTESIAN_POINT('Ctrl Pts',(-14.5008952119779,5.15081623233879,-19.0450824562991));
#17704=CARTESIAN_POINT('Ctrl Pts',(-14.4931017851657,5.16101344797881,-19.1473283610123));
#17705=CARTESIAN_POINT('Ctrl Pts',(-14.4888014238203,5.16614762734179,-19.1889301853698));
#17706=CARTESIAN_POINT('Ctrl Pts',(-14.4769322259441,5.17896676324241,-19.2616359812616));
#17707=CARTESIAN_POINT('Ctrl Pts',(-14.4720622413096,5.18410167008481,-19.287578866658));
#17708=CARTESIAN_POINT('Ctrl Pts',(-14.4629416839796,5.19347468131139,-19.3288153342604));
#17709=CARTESIAN_POINT('Ctrl Pts',(-14.4579266625362,5.19857937379608,-19.35001262557));
#17710=CARTESIAN_POINT('Ctrl Pts',(-14.4511743173673,5.20535340038314,-19.3756863417983));
#17711=CARTESIAN_POINT('Ctrl Pts',(-14.4480754803313,5.20844138893622,-19.3868828151978));
#17712=CARTESIAN_POINT('Ctrl Pts',(-14.4459627179149,5.21054216771168,-19.3943891095122));
#17713=CARTESIAN_POINT('Ctrl Pts',(-14.4444040881137,5.21208770973309,-19.3998091262346));
#17714=CARTESIAN_POINT('Ctrl Pts',(-14.4237756906843,5.23251270441264,-19.470717215959));
#17715=CARTESIAN_POINT('Ctrl Pts',(-14.3993690637851,5.25635306321645,-19.5340649358218));
#17716=CARTESIAN_POINT('Ctrl Pts',(-14.3583270196641,5.29682852688184,-19.6201464487895));
#17717=CARTESIAN_POINT('Ctrl Pts',(-14.3439056403182,5.31110495308435,-19.6473572697992));
#17718=CARTESIAN_POINT('Ctrl Pts',(-14.3139153763737,5.34099752748566,-19.6987524160761));
#17719=CARTESIAN_POINT('Ctrl Pts',(-14.2976357723532,5.3573325510963,-19.7239445600959));
#17720=CARTESIAN_POINT('Ctrl Pts',(-14.251808341393,5.40369189151976,-19.788911112043));
#17721=CARTESIAN_POINT('Ctrl Pts',(-14.2168974150654,5.43964379893236,-19.8306766770307));
#17722=CARTESIAN_POINT('Ctrl Pts',(-14.1571767183151,5.5017717037822,-19.8879120782552));
#17723=CARTESIAN_POINT('Ctrl Pts',(-14.13604578679,5.52383933229555,-19.9060806952842));
#17724=CARTESIAN_POINT('Ctrl Pts',(-14.091226182727,5.57066956248382,-19.9400003402937));
#17725=CARTESIAN_POINT('Ctrl Pts',(-14.0688649668062,5.59405032517479,-19.9549959653081));
#17726=CARTESIAN_POINT('Ctrl Pts',(-13.9898492875009,5.67633337742647,-19.9999263838268));
#17727=CARTESIAN_POINT('Ctrl Pts',(-13.938482954597,5.7289080828448,-20.0192563633749));
#17728=CARTESIAN_POINT('Ctrl Pts',(-13.8667310709799,5.8014471380659,-20.0371046073501));
#17729=CARTESIAN_POINT('Ctrl Pts',(-13.8436826949468,5.82459789936379,-20.0411970669116));
#17730=CARTESIAN_POINT('Ctrl Pts',(-13.8107160108327,5.85760768308144,-20.0451193489524));
#17731=CARTESIAN_POINT('Ctrl Pts',(-13.7946330526942,5.87368517909651,-20.0465257906122));
#17732=CARTESIAN_POINT('Ctrl Pts',(-13.776625690848,5.89167240033343,-20.0473128143698));
#17733=CARTESIAN_POINT('Ctrl Pts',(-13.7690755742853,5.89921476072116,-20.0474791032041));
#17734=CARTESIAN_POINT('Ctrl Pts',(-13.7640799210943,5.90420586521239,-20.0475532708907));
#17735=CARTESIAN_POINT('Ctrl Pts',(-13.7625698364558,5.90571455194702,-20.0475716004378));
#17736=CARTESIAN_POINT('Ctrl Pts',(-13.6494244217083,6.01879388001767,-20.0476194900863));
#17737=CARTESIAN_POINT('Ctrl Pts',(-13.5458171256965,6.12076447135899,-20.0142261657798));
#17738=CARTESIAN_POINT('Ctrl Pts',(-13.4098535901725,6.25310609308376,-19.9326926928262));
#17739=CARTESIAN_POINT('Ctrl Pts',(-13.3676863827449,6.29390535776389,-19.9002696352502));
#17740=CARTESIAN_POINT('Ctrl Pts',(-13.309816922612,6.34986186513291,-19.8458099780658));
#17741=CARTESIAN_POINT('Ctrl Pts',(-13.2914204068164,6.36764506169195,-19.8266825482732));
#17742=CARTESIAN_POINT('Ctrl Pts',(-13.2652190679446,6.39301754356787,-19.7967518928305));
#17743=CARTESIAN_POINT('Ctrl Pts',(-13.2567173583171,6.40125818545505,-19.7865681729864));
#17744=CARTESIAN_POINT('Ctrl Pts',(-13.2401851344379,6.41730803640871,-19.7658209853051));
#17745=CARTESIAN_POINT('Ctrl Pts',(-13.2329761306639,6.42431648236243,-19.7563895777018));
#17746=CARTESIAN_POINT('Ctrl Pts',(-13.1899088809362,6.46629626026074,-19.6970422219169));
#17747=CARTESIAN_POINT('Ctrl Pts',(-13.1591326285648,6.49695931139492,-19.6442998690099));
#17748=CARTESIAN_POINT('Ctrl Pts',(-13.1187018339531,6.5375766182669,-19.5583253785774));
#17749=CARTESIAN_POINT('Ctrl Pts',(-13.1061787094182,6.5502185564322,-19.528522650004));
#17750=CARTESIAN_POINT('Ctrl Pts',(-13.0830590576994,6.57352678897084,-19.4667920197417));
#17751=CARTESIAN_POINT('Ctrl Pts',(-13.0729825680116,6.5836755636959,-19.4366418158537));
#17752=CARTESIAN_POINT('Ctrl Pts',(-13.0222431195477,6.63416909254319,-19.263206741482));
#17753=CARTESIAN_POINT('Ctrl Pts',(-13.0012748264626,6.65,-19.1269039490329));
#17754=CARTESIAN_POINT('Ctrl Pts',(-13.,6.65000000000009,-18.9999999999985));
#17755=CARTESIAN_POINT('Origin',(-13.,-34.65,-19.));
#17756=CARTESIAN_POINT('Ctrl Pts',(-13.,-36.15,-19.));
#17757=CARTESIAN_POINT('Ctrl Pts',(-13.0022600019962,-36.15,-19.0595135681354));
#17758=CARTESIAN_POINT('Ctrl Pts',(-13.0073620228199,-36.1464573811096,
-19.118348117267));
#17759=CARTESIAN_POINT('Ctrl Pts',(-13.0153053530567,-36.1395493826994,
-19.1760919721841));
#17760=CARTESIAN_POINT('Ctrl Pts',(-13.0166707573576,-36.1383619448793,
-19.1860177470804));
#17761=CARTESIAN_POINT('Ctrl Pts',(-13.0181201082012,-36.1370749459201,
-19.1959113155705));
#17762=CARTESIAN_POINT('Ctrl Pts',(-13.019653390988,-36.1356891362019,-19.2057705877774));
#17763=CARTESIAN_POINT('Ctrl Pts',(-13.0232674597517,-36.1324226731215,
-19.2290096719323));
#17764=CARTESIAN_POINT('Ctrl Pts',(-13.0272781780458,-36.1286470144162,
-19.2518093520673));
#17765=CARTESIAN_POINT('Ctrl Pts',(-13.0317575007099,-36.1243454280086,
-19.2744030248717));
#17766=CARTESIAN_POINT('Ctrl Pts',(-13.0362018078249,-36.1200774677586,
-19.2968200794869));
#17767=CARTESIAN_POINT('Ctrl Pts',(-13.0411074346003,-36.115291625118,-19.31903476708));
#17768=CARTESIAN_POINT('Ctrl Pts',(-13.0465443279275,-36.1099219905614,
-19.3412644238901));
#17769=CARTESIAN_POINT('Ctrl Pts',(-13.051477160096,-36.105050181519,-19.3614331415028));
#17770=CARTESIAN_POINT('Ctrl Pts',(-13.0568473243463,-36.0996972429254,
-19.381614336502));
#17771=CARTESIAN_POINT('Ctrl Pts',(-13.0627066489669,-36.0937789851613,
-19.4019578562263));
#17772=CARTESIAN_POINT('Ctrl Pts',(-13.0781595750661,-36.0781706333824,
-19.4556102696443));
#17773=CARTESIAN_POINT('Ctrl Pts',(-13.0962876949103,-36.0596294661765,
-19.5068516934339));
#17774=CARTESIAN_POINT('Ctrl Pts',(-13.1170615404837,-36.038502108525,-19.5553003604907));
#17775=CARTESIAN_POINT('Ctrl Pts',(-13.1215965043751,-36.0338899723786,
-19.5658767824108));
#17776=CARTESIAN_POINT('Ctrl Pts',(-13.1262574478772,-36.0291544387819,
-19.5763200414124));
#17777=CARTESIAN_POINT('Ctrl Pts',(-13.1310438701045,-36.0242988849141,
-19.586626012918));
#17778=CARTESIAN_POINT('Ctrl Pts',(-13.1443999464778,-36.0107499029783,
-19.6153838900956));
#17779=CARTESIAN_POINT('Ctrl Pts',(-13.1587334900227,-35.9962665987231,
-19.6430731920865));
#17780=CARTESIAN_POINT('Ctrl Pts',(-13.1740297517348,-35.9809201189384,
-19.6696008381985));
#17781=CARTESIAN_POINT('Ctrl Pts',(-13.1816778825908,-35.9732468790461,
-19.6828646612545));
#17782=CARTESIAN_POINT('Ctrl Pts',(-13.1895666820908,-35.9653577656181,
-19.6958380292842));
#17783=CARTESIAN_POINT('Ctrl Pts',(-13.1976935757629,-35.9572615166724,
-19.7085086994028));
#17784=CARTESIAN_POINT('Ctrl Pts',(-13.201757022599,-35.9532133921996,-19.7148440344621));
#17785=CARTESIAN_POINT('Ctrl Pts',(-13.2058799925016,-35.9491134795596,
-19.7211036930482));
#17786=CARTESIAN_POINT('Ctrl Pts',(-13.2100621289874,-35.9449628612145,
-19.727286112916));
#17787=CARTESIAN_POINT('Ctrl Pts',(-13.2129317585397,-35.942114858261,-19.7315282639834));
#17788=CARTESIAN_POINT('Ctrl Pts',(-13.2161072666263,-35.9389722558302,
-19.7361264257704));
#17789=CARTESIAN_POINT('Ctrl Pts',(-13.2190161563155,-35.9360911505925,
-19.7402712176227));
#17790=CARTESIAN_POINT('Ctrl Pts',(-13.2203466199925,-35.9347733949269,
-19.7421669564088));
#17791=CARTESIAN_POINT('Ctrl Pts',(-13.2216213369746,-35.9335109849067,
-19.7439683311337));
#17792=CARTESIAN_POINT('Ctrl Pts',(-13.2227856645689,-35.9323599620334,
-19.7456000774117));
#17793=CARTESIAN_POINT('Ctrl Pts',(-13.2405637498969,-35.9147850261165,
-19.770515165491));
#17794=CARTESIAN_POINT('Ctrl Pts',(-13.2598640476502,-35.8959665645779,
-19.7946098108024));
#17795=CARTESIAN_POINT('Ctrl Pts',(-13.2806405457828,-35.875849115071,-19.8176397930277));
#17796=CARTESIAN_POINT('Ctrl Pts',(-13.3008006762476,-35.8563284815124,
-19.8399865544164));
#17797=CARTESIAN_POINT('Ctrl Pts',(-13.3223509769984,-35.8355841698481,
-19.8613306716612));
#17798=CARTESIAN_POINT('Ctrl Pts',(-13.3452294106231,-35.8135863624122,
-19.8814099110228));
#17799=CARTESIAN_POINT('Ctrl Pts',(-13.3680574656225,-35.7916369944506,
-19.9014449356234));
#17800=CARTESIAN_POINT('Ctrl Pts',(-13.3922081788925,-35.7684389191712,
-19.9202204461223));
#17801=CARTESIAN_POINT('Ctrl Pts',(-13.4175949294794,-35.7439937052078,
-19.9374391968756));
#17802=CARTESIAN_POINT('Ctrl Pts',(-13.4413843218865,-35.721086607056,-19.9535745276667));
#17803=CARTESIAN_POINT('Ctrl Pts',(-13.4662591457732,-35.6970841490617,
-19.9683422449517));
#17804=CARTESIAN_POINT('Ctrl Pts',(-13.4921236616887,-35.6720212156899,
-19.9814718214427));
#17805=CARTESIAN_POINT('Ctrl Pts',(-13.5174413758654,-35.6474881377999,
-19.9943238255531));
#17806=CARTESIAN_POINT('Ctrl Pts',(-13.5437075604159,-35.6219385906434,
-20.0056057520444));
#17807=CARTESIAN_POINT('Ctrl Pts',(-13.5708063058782,-35.5954430912409,
-20.0150455765111));
#17808=CARTESIAN_POINT('Ctrl Pts',(-13.5971431852752,-35.5696924979781,
-20.024220005595));
#17809=CARTESIAN_POINT('Ctrl Pts',(-13.6242665787865,-35.5430481880217,
-20.0316539195612));
#17810=CARTESIAN_POINT('Ctrl Pts',(-13.652043084933,-35.515615010231,-20.0370874936349));
#17811=CARTESIAN_POINT('Ctrl Pts',(-13.6599625404285,-35.5077934422674,
-20.0386366786848));
#17812=CARTESIAN_POINT('Ctrl Pts',(-13.6679349096542,-35.4999080132942,
-20.0400232205253));
#17813=CARTESIAN_POINT('Ctrl Pts',(-13.6759566644634,-35.4919618070296,
-20.0412410399475));
#17814=CARTESIAN_POINT('Ctrl Pts',(-13.689561502004,-35.4784850992684,-20.0433064527889));
#17815=CARTESIAN_POINT('Ctrl Pts',(-13.7033084869127,-35.4648334295818,
-20.0448865414506));
#17816=CARTESIAN_POINT('Ctrl Pts',(-13.7171790381733,-35.4510238866596,
-20.045951700704));
#17817=CARTESIAN_POINT('Ctrl Pts',(-13.7241143138036,-35.4441191151985,
-20.0464842803307));
#17818=CARTESIAN_POINT('Ctrl Pts',(-13.7310804857771,-35.4371748806365,
-20.0468881344733));
#17819=CARTESIAN_POINT('Ctrl Pts',(-13.7380750284009,-35.4301936070775,
-20.0471595809266));
#17820=CARTESIAN_POINT('Ctrl Pts',(-13.7415722997128,-35.4267029702981,
-20.0472953041532));
#17821=CARTESIAN_POINT('Ctrl Pts',(-13.7450766640841,-35.4232030742188,
-20.0473979260404));
#17822=CARTESIAN_POINT('Ctrl Pts',(-13.7485878000069,-35.4196942321784,
-20.0474669897578));
#17823=CARTESIAN_POINT('Ctrl Pts',(-13.7512425760978,-35.417041190496,-20.0475192089568));
#17824=CARTESIAN_POINT('Ctrl Pts',(-13.754398814031,-35.4138864585152,-20.047555584487));
#17825=CARTESIAN_POINT('Ctrl Pts',(-13.7569273746134,-35.41135644911,-20.0475673281272));
#17826=CARTESIAN_POINT('Ctrl Pts',(-13.7577430206946,-35.4105403356773,
-20.0475711163117));
#17827=CARTESIAN_POINT('Ctrl Pts',(-13.7584934884378,-35.4097892758672,
-20.0475727773388));
#17828=CARTESIAN_POINT('Ctrl Pts',(-13.7591411982523,-35.409141187524,-20.0475730516392));
#17829=CARTESIAN_POINT('Ctrl Pts',(-13.7804931212359,-35.3877767862455,
-20.0475820940239));
#17830=CARTESIAN_POINT('Ctrl Pts',(-13.8026529826069,-35.3656086503563,
-20.0462820505238));
#17831=CARTESIAN_POINT('Ctrl Pts',(-13.8254839292651,-35.3427124028573,
-20.0434202458515));
#17832=CARTESIAN_POINT('Ctrl Pts',(-13.8481437806401,-35.3199877400064,
-20.0405798875646));
#17833=CARTESIAN_POINT('Ctrl Pts',(-13.8714648759401,-35.2965453990989,
-20.0362005538921));
#17834=CARTESIAN_POINT('Ctrl Pts',(-13.8952849871958,-35.2725025402055,
-20.0300268827267));
#17835=CARTESIAN_POINT('Ctrl Pts',(-13.9191050984514,-35.248459681312,-20.0238532115612));
#17836=CARTESIAN_POINT('Ctrl Pts',(-13.9434244184388,-35.2238158694878,
-20.0158845175589));
#17837=CARTESIAN_POINT('Ctrl Pts',(-13.9680493372299,-35.1987382984234,
-20.0058661742659));
#17838=CARTESIAN_POINT('Ctrl Pts',(-13.977457672413,-35.1891570203629,-20.002038509595));
#17839=CARTESIAN_POINT('Ctrl Pts',(-13.9871299309948,-35.1792932147603,
-19.9978150359244));
#17840=CARTESIAN_POINT('Ctrl Pts',(-13.9967972145168,-35.1694120988939,
-19.993280617275));
#17841=CARTESIAN_POINT('Ctrl Pts',(-14.0064058021206,-35.1595909772509,
-19.9887737298204));
#17842=CARTESIAN_POINT('Ctrl Pts',(-14.0160093075113,-35.1497530912975,
-19.9839596558358));
#17843=CARTESIAN_POINT('Ctrl Pts',(-14.0253653094095,-35.1401498665673,
-19.9789683807783));
#17844=CARTESIAN_POINT('Ctrl Pts',(-14.0312956955279,-35.1340627760288,
-19.9758046161023));
#17845=CARTESIAN_POINT('Ctrl Pts',(-14.0371270970296,-35.1280697608133,
-19.9725706227735));
#17846=CARTESIAN_POINT('Ctrl Pts',(-14.0428025582102,-35.122232141555,-19.9693088409132));
#17847=CARTESIAN_POINT('Ctrl Pts',(-14.0701611976502,-35.0940918168496,
-19.9535853761576));
#17848=CARTESIAN_POINT('Ctrl Pts',(-14.0963327095386,-35.0670311408392,
-19.9358471136705));
#17849=CARTESIAN_POINT('Ctrl Pts',(-14.1212830788775,-35.0411979198204,
-19.9163451557962));
#17850=CARTESIAN_POINT('Ctrl Pts',(-14.1394468349885,-35.0223914516768,
-19.9021478186064));
#17851=CARTESIAN_POINT('Ctrl Pts',(-14.1569636554044,-35.0042343822968,
-19.887016043089));
#17852=CARTESIAN_POINT('Ctrl Pts',(-14.1738240977961,-34.986766893543,-19.8710482459925));
#17853=CARTESIAN_POINT('Ctrl Pts',(-14.193834365055,-34.966036173068,-19.8520973857473));
#17854=CARTESIAN_POINT('Ctrl Pts',(-14.212919974189,-34.946277284871,-19.8319691573682));
#17855=CARTESIAN_POINT('Ctrl Pts',(-14.2310705495146,-34.9275330934599,
-19.8108271604679));
#17856=CARTESIAN_POINT('Ctrl Pts',(-14.2401458371774,-34.9181609977544,
-19.8002561620177));
#17857=CARTESIAN_POINT('Ctrl Pts',(-14.2489874564823,-34.9090421748539,
-19.7894316869711));
#17858=CARTESIAN_POINT('Ctrl Pts',(-14.2575946377114,-34.9001796687312,
-19.7783738565453));
#17859=CARTESIAN_POINT('Ctrl Pts',(-14.2618982283259,-34.8957484156699,
-19.7728449413323));
#17860=CARTESIAN_POINT('Ctrl Pts',(-14.2663517713433,-34.8911685633083,
-19.7669825101925));
#17861=CARTESIAN_POINT('Ctrl Pts',(-14.2706384453579,-34.8867626882363,
-19.7611973270037));
#17862=CARTESIAN_POINT('Ctrl Pts',(-14.2749251193725,-34.8823568131644,
-19.7554121438149));
#17863=CARTESIAN_POINT('Ctrl Pts',(-14.2790451446463,-34.8781247953313,
-19.7497046604211));
#17864=CARTESIAN_POINT('Ctrl Pts',(-14.2827124379421,-34.8743626807183,
-19.7445201065448));
#17865=CARTESIAN_POINT('Ctrl Pts',(-14.2975068311467,-34.8591857645633,
-19.723604864035));
#17866=CARTESIAN_POINT('Ctrl Pts',(-14.3123312731224,-34.8441459052951,
-19.7008120823653));
#17867=CARTESIAN_POINT('Ctrl Pts',(-14.3269411121185,-34.8294304558811,
-19.6760414162402));
#17868=CARTESIAN_POINT('Ctrl Pts',(-14.3413036352122,-34.8149641101464,
-19.65169006888));
#17869=CARTESIAN_POINT('Ctrl Pts',(-14.3554586875722,-34.800811416631,-19.6254266232903));
#17870=CARTESIAN_POINT('Ctrl Pts',(-14.3691431631417,-34.7871752343393,
-19.5971850248509));
#17871=CARTESIAN_POINT('Ctrl Pts',(-14.377964125389,-34.77838540176,-19.5789805951401));
#17872=CARTESIAN_POINT('Ctrl Pts',(-14.3865034952691,-34.7698922778293,
-19.5601396048537));
#17873=CARTESIAN_POINT('Ctrl Pts',(-14.3947786435268,-34.761666544262,-19.5404841518991));
#17874=CARTESIAN_POINT('Ctrl Pts',(-14.402873396153,-34.7536201291014,-19.5212571816421));
#17875=CARTESIAN_POINT('Ctrl Pts',(-14.4107155303935,-34.745829345794,-19.5012505138998));
#17876=CARTESIAN_POINT('Ctrl Pts',(-14.4182846912925,-34.7382967410889,
-19.4802834787482));
#17877=CARTESIAN_POINT('Ctrl Pts',(-14.4255810866987,-34.7310355845221,
-19.460072020569));
#17878=CARTESIAN_POINT('Ctrl Pts',(-14.432623973438,-34.7240141747685,-19.438967780527));
#17879=CARTESIAN_POINT('Ctrl Pts',(-14.4393582806655,-34.7172656557504,
-19.416800997403));
#17880=CARTESIAN_POINT('Ctrl Pts',(-14.4408457714661,-34.7157750258135,
-19.4119047423225));
#17881=CARTESIAN_POINT('Ctrl Pts',(-14.442318054546,-34.7142978388433,-19.4069566280643));
#17882=CARTESIAN_POINT('Ctrl Pts',(-14.4437742694652,-34.7128346783188,
-19.4019548009798));
#17883=CARTESIAN_POINT('Ctrl Pts',(-14.4516573515213,-34.704913996884,-19.3748778820325));
#17884=CARTESIAN_POINT('Ctrl Pts',(-14.4582965001819,-34.6980624380417,
-19.3489100616057));
#17885=CARTESIAN_POINT('Ctrl Pts',(-14.4639363715387,-34.6921184214563,
-19.3242164996728));
#17886=CARTESIAN_POINT('Ctrl Pts',(-14.4661232996319,-34.689813557385,-19.3146412734141));
#17887=CARTESIAN_POINT('Ctrl Pts',(-14.4681597602534,-34.6876451182921,
-19.3052571195871));
#17888=CARTESIAN_POINT('Ctrl Pts',(-14.4700591413543,-34.6856036616695,
-19.2960717821684));
#17889=CARTESIAN_POINT('Ctrl Pts',(-14.4734579899498,-34.6819505759507,
-19.2796350748798));
#17890=CARTESIAN_POINT('Ctrl Pts',(-14.4764182288969,-34.6787040153216,
-19.2638355067169));
#17891=CARTESIAN_POINT('Ctrl Pts',(-14.4790122221135,-34.675810656934,-19.2487099853794));
#17892=CARTESIAN_POINT('Ctrl Pts',(-14.4803092187218,-34.6743639777403,
-19.2411472247106));
#17893=CARTESIAN_POINT('Ctrl Pts',(-14.4815145444226,-34.6730055973423,
-19.2337529581117));
#17894=CARTESIAN_POINT('Ctrl Pts',(-14.4826367188746,-34.6717290413985,
-19.2265308116014));
#17895=CARTESIAN_POINT('Ctrl Pts',(-14.4833342253485,-34.6709355765022,
-19.2220417645213));
#17896=CARTESIAN_POINT('Ctrl Pts',(-14.4839235679003,-34.6702614216444,
-19.2181274908503));
#17897=CARTESIAN_POINT('Ctrl Pts',(-14.4845504271016,-34.6695394891977,
-19.2138416183871));
#17898=CARTESIAN_POINT('Ctrl Pts',(-14.4849320823828,-34.6690999497757,
-19.2112322192478));
#17899=CARTESIAN_POINT('Ctrl Pts',(-14.4853270789114,-34.6686432749335,
-19.2084849023242));
#17900=CARTESIAN_POINT('Ctrl Pts',(-14.4857618520254,-34.6681384289453,
-19.2053843140591));
#17901=CARTESIAN_POINT('Ctrl Pts',(-14.4877126337078,-34.6658732375746,
-19.1914722974293));
#17902=CARTESIAN_POINT('Ctrl Pts',(-14.4895157198301,-34.6637373060712,
-19.1771171773623));
#17903=CARTESIAN_POINT('Ctrl Pts',(-14.491111562952,-34.6618111725586,-19.1626247306949));
#17904=CARTESIAN_POINT('Ctrl Pts',(-14.4926914399074,-34.6599043097174,
-19.148277278741));
#17905=CARTESIAN_POINT('Ctrl Pts',(-14.4940681658665,-34.6582032367635,
-19.133795531894));
#17906=CARTESIAN_POINT('Ctrl Pts',(-14.495218285289,-34.656748536048,-19.1194852986711));
#17907=CARTESIAN_POINT('Ctrl Pts',(-14.4956431709154,-34.656211129747,-19.1141987064384));
#17908=CARTESIAN_POINT('Ctrl Pts',(-14.496037470133,-34.6557069655761,-19.1089355887219));
#17909=CARTESIAN_POINT('Ctrl Pts',(-14.4964011799049,-34.6552367471062,
-19.1037115483395));
#17910=CARTESIAN_POINT('Ctrl Pts',(-14.4971421310599,-34.6542788159608,
-19.0930691101825));
#17911=CARTESIAN_POINT('Ctrl Pts',(-14.4977897720911,-34.6534179560291,
-19.0820681263714));
#17912=CARTESIAN_POINT('Ctrl Pts',(-14.4983114928388,-34.6526999839116,
-19.0711011991041));
#17913=CARTESIAN_POINT('Ctrl Pts',(-14.4986145484379,-34.6522829303995,
-19.0647307629515));
#17914=CARTESIAN_POINT('Ctrl Pts',(-14.4988757501221,-34.6519133677684,
-19.0583719341073));
#17915=CARTESIAN_POINT('Ctrl Pts',(-14.4990939964136,-34.6515941473328,
-19.052102289881));
#17916=CARTESIAN_POINT('Ctrl Pts',(-14.4993692024711,-34.6511916140436,
-19.044196340793));
#17917=CARTESIAN_POINT('Ctrl Pts',(-14.4995892882439,-34.6508491822811,
-19.0359873571226));
#17918=CARTESIAN_POINT('Ctrl Pts',(-14.4997384781478,-34.6505922042186,
-19.028002615185));
#17919=CARTESIAN_POINT('Ctrl Pts',(-14.499750283177,-34.6505718701782,-19.0273708022445));
#17920=CARTESIAN_POINT('Ctrl Pts',(-14.4997616618496,-34.6505520505088,
-19.0267403944298));
#17921=CARTESIAN_POINT('Ctrl Pts',(-14.4997726153437,-34.6505327471463,
-19.0261116534472));
#17922=CARTESIAN_POINT('Ctrl Pts',(-14.4998099608049,-34.6504669331722,
-19.0239679884345));
#17923=CARTESIAN_POINT('Ctrl Pts',(-14.4998429628733,-34.6504060666365,
-19.0218093966219));
#17924=CARTESIAN_POINT('Ctrl Pts',(-14.4998714305716,-34.6503504002792,
-19.0196359103402));
#17925=CARTESIAN_POINT('Ctrl Pts',(-14.4998913569453,-34.6503114358138,
-19.0181145474362));
#17926=CARTESIAN_POINT('Ctrl Pts',(-14.4998972483018,-34.6502995823162,
-19.0176308556723));
#17927=CARTESIAN_POINT('Ctrl Pts',(-14.4999147420331,-34.6502622818368,
-19.0159905547103));
#17928=CARTESIAN_POINT('Ctrl Pts',(-14.4999222406195,-34.6502462932029,
-19.0152874492243));
#17929=CARTESIAN_POINT('Ctrl Pts',(-14.499931696151,-34.6502258364736,-19.0143718256226));
#17930=CARTESIAN_POINT('Ctrl Pts',(-14.499943037045,-34.6501992580938,-19.0130708039746));
#17931=CARTESIAN_POINT('Ctrl Pts',(-14.4999813878725,-34.650109379565,-19.0086712163251));
#17932=CARTESIAN_POINT('Ctrl Pts',(-14.4999919153336,-34.6500539914906,
-19.0053844415825));
#17933=CARTESIAN_POINT('Ctrl Pts',(-14.4999965710807,-34.6500280644066,
-19.0032071730045));
#17934=CARTESIAN_POINT('Ctrl Pts',(-14.5000010927208,-34.6500028841417,
-19.001092619763));
#17935=CARTESIAN_POINT('Ctrl Pts',(-14.5,-34.6500001237228,-19.0000246345907));
#17936=CARTESIAN_POINT('Ctrl Pts',(-14.5,-34.65,-19.));
#17937=CARTESIAN_POINT('Origin',(-6.65,-41.,-19.));
#17938=CARTESIAN_POINT('Ctrl Pts',(-6.65,-42.5,-18.9999999999996));
#17939=CARTESIAN_POINT('Ctrl Pts',(-6.65226000199757,-42.5,-19.0595135681296));
#17940=CARTESIAN_POINT('Ctrl Pts',(-6.65736202282211,-42.4964573811102,
-19.1183481172583));
#17941=CARTESIAN_POINT('Ctrl Pts',(-6.66530535305908,-42.4895493827004,
-19.1760919721752));
#17942=CARTESIAN_POINT('Ctrl Pts',(-6.66667075735998,-42.4883619448805,
-19.1860177470708));
#17943=CARTESIAN_POINT('Ctrl Pts',(-6.66812010820348,-42.4870749459215,
-19.1959113155602));
#17944=CARTESIAN_POINT('Ctrl Pts',(-6.66965339099016,-42.4856891362034,
-19.2057705877665));
#17945=CARTESIAN_POINT('Ctrl Pts',(-6.67326745976708,-42.4824226731111,
-19.2290096720071));
#17946=CARTESIAN_POINT('Ctrl Pts',(-6.67727817807838,-42.4786470143895,
-19.2518093522287));
#17947=CARTESIAN_POINT('Ctrl Pts',(-6.68175750076314,-42.4743454279614,
-19.2744030251193));
#17948=CARTESIAN_POINT('Ctrl Pts',(-6.68620180789899,-42.4700774676907,
-19.2968200798215));
#17949=CARTESIAN_POINT('Ctrl Pts',(-6.69110743469881,-42.4652916250251,
-19.319034767501));
#17950=CARTESIAN_POINT('Ctrl Pts',(-6.69654432805367,-42.4599219904392,
-19.3412644243957));
#17951=CARTESIAN_POINT('Ctrl Pts',(-6.70147716018822,-42.4550501814286,
-19.3614331418438));
#17952=CARTESIAN_POINT('Ctrl Pts',(-6.70684732439677,-42.4496972428746,
-19.3816143366766));
#17953=CARTESIAN_POINT('Ctrl Pts',(-6.71270664896581,-42.4437789851613,
-19.4019578562263));
#17954=CARTESIAN_POINT('Ctrl Pts',(-6.72815957505023,-42.4281706333941,
-19.4556102696049));
#17955=CARTESIAN_POINT('Ctrl Pts',(-6.74628769488154,-42.409629466202,-19.5068516933656));
#17956=CARTESIAN_POINT('Ctrl Pts',(-6.76706154044398,-42.3885021085632,
-19.5553003604037));
#17957=CARTESIAN_POINT('Ctrl Pts',(-6.77159650434243,-42.3838899724099,
-19.5658767823418));
#17958=CARTESIAN_POINT('Ctrl Pts',(-6.77625744785224,-42.3791544388057,
-19.5763200413613));
#17959=CARTESIAN_POINT('Ctrl Pts',(-6.78104387008779,-42.3742988849298,
-19.5866260128848));
#17960=CARTESIAN_POINT('Ctrl Pts',(-6.79439994646144,-42.3607499029948,
-19.6153838900628));
#17961=CARTESIAN_POINT('Ctrl Pts',(-6.80873349000797,-42.3462665987391,
-19.6430731920569));
#17962=CARTESIAN_POINT('Ctrl Pts',(-6.82402975172317,-42.330920118952,-19.6696008381745));
#17963=CARTESIAN_POINT('Ctrl Pts',(-6.83167788258077,-42.3232468790584,
-19.6828646612334));
#17964=CARTESIAN_POINT('Ctrl Pts',(-6.83956668208268,-42.3153577656287,
-19.6958380292666));
#17965=CARTESIAN_POINT('Ctrl Pts',(-6.847693575757,-42.3072615166807,-19.7085086993891));
#17966=CARTESIAN_POINT('Ctrl Pts',(-6.85175702259416,-42.3032133922067,
-19.7148440344504));
#17967=CARTESIAN_POINT('Ctrl Pts',(-6.85587999249803,-42.2991134795655,
-19.7211036930386));
#17968=CARTESIAN_POINT('Ctrl Pts',(-6.86006212898514,-42.294962861219,-19.7272861129087));
#17969=CARTESIAN_POINT('Ctrl Pts',(-6.86293175853638,-42.2921148582665,
-19.7315282639747));
#17970=CARTESIAN_POINT('Ctrl Pts',(-6.86610726662219,-42.2889722558363,
-19.736126425761));
#17971=CARTESIAN_POINT('Ctrl Pts',(-6.86901615631067,-42.2860911505991,
-19.7402712176126));
#17972=CARTESIAN_POINT('Ctrl Pts',(-6.87034661999027,-42.2847733949309,
-19.7421669564025));
#17973=CARTESIAN_POINT('Ctrl Pts',(-6.87162133697474,-42.2835109849082,
-19.7439683311309));
#17974=CARTESIAN_POINT('Ctrl Pts',(-6.87278566457079,-42.2823599620331,
-19.7456000774116));
#17975=CARTESIAN_POINT('Ctrl Pts',(-6.89056374990032,-42.2647850261135,
-19.7705151654949));
#17976=CARTESIAN_POINT('Ctrl Pts',(-6.90986404765536,-42.2459665645722,
-19.7946098108098));
#17977=CARTESIAN_POINT('Ctrl Pts',(-6.93064054578988,-42.2258491150625,
-19.8176397930381));
#17978=CARTESIAN_POINT('Ctrl Pts',(-6.95080067625634,-42.2063284815013,
-19.8399865544295));
#17979=CARTESIAN_POINT('Ctrl Pts',(-6.97235097700896,-42.1855841698343,
-19.8613306716764));
#17980=CARTESIAN_POINT('Ctrl Pts',(-6.99522941063554,-42.1635863623958,
-19.8814099110395));
#17981=CARTESIAN_POINT('Ctrl Pts',(-7.01805746563467,-42.1416369944338,
-19.9014449356397));
#17982=CARTESIAN_POINT('Ctrl Pts',(-7.04220817890412,-42.1184389191542,
-19.920220446138));
#17983=CARTESIAN_POINT('Ctrl Pts',(-7.06759492949033,-42.093993705191,-19.9374391968903));
#17984=CARTESIAN_POINT('Ctrl Pts',(-7.0913843218999,-42.0710866070363,-19.9535745276827));
#17985=CARTESIAN_POINT('Ctrl Pts',(-7.1162591457892,-42.0470841490393,-19.9683422449684));
#17986=CARTESIAN_POINT('Ctrl Pts',(-7.14212366170743,-42.0220212156647,
-19.9814718214594));
#17987=CARTESIAN_POINT('Ctrl Pts',(-7.16744137588612,-41.9974881377729,
-19.9943238255695));
#17988=CARTESIAN_POINT('Ctrl Pts',(-7.19370756043867,-41.9719385906145,
-20.0056057520601));
#17989=CARTESIAN_POINT('Ctrl Pts',(-7.22080630590297,-41.9454430912103,
-20.0150455765255));
#17990=CARTESIAN_POINT('Ctrl Pts',(-7.24714318530013,-41.9196924979478,
-20.0242200056076));
#17991=CARTESIAN_POINT('Ctrl Pts',(-7.27426657881137,-41.8930481879919,
-20.0316539195719));
#17992=CARTESIAN_POINT('Ctrl Pts',(-7.30204308495783,-41.865615010202,-20.0370874936434));
#17993=CARTESIAN_POINT('Ctrl Pts',(-7.30996254044553,-41.8577934422464,
-20.0386366786911));
#17994=CARTESIAN_POINT('Ctrl Pts',(-7.31793490966327,-41.8499080132814,
-20.0400232205299));
#17995=CARTESIAN_POINT('Ctrl Pts',(-7.32595666446443,-41.841961807025,-20.0412410399506));
#17996=CARTESIAN_POINT('Ctrl Pts',(-7.33956150200486,-41.8284850992645,
-20.0433064527914));
#17997=CARTESIAN_POINT('Ctrl Pts',(-7.35330848691337,-41.8148334295786,
-20.0448865414527));
#17998=CARTESIAN_POINT('Ctrl Pts',(-7.36717903817378,-41.8010238866572,
-20.0459517007055));
#17999=CARTESIAN_POINT('Ctrl Pts',(-7.37411431380399,-41.7941191151964,
-20.0464842803319));
#18000=CARTESIAN_POINT('Ctrl Pts',(-7.38108048577737,-41.7871748806348,
-20.0468881344744));
#18001=CARTESIAN_POINT('Ctrl Pts',(-7.38807502840106,-41.7801936070763,
-20.0471595809274));
#18002=CARTESIAN_POINT('Ctrl Pts',(-7.3915722997129,-41.7767029702971,-20.0472953041539));
#18003=CARTESIAN_POINT('Ctrl Pts',(-7.39507666408421,-41.773203074218,-20.0473979260409));
#18004=CARTESIAN_POINT('Ctrl Pts',(-7.39858780000693,-41.7696942321778,
-20.0474669897582));
#18005=CARTESIAN_POINT('Ctrl Pts',(-7.40124257609955,-41.7670411904938,
-20.0475192089572));
#18006=CARTESIAN_POINT('Ctrl Pts',(-7.40439881403369,-41.7638864585122,
-20.0475555844873));
#18007=CARTESIAN_POINT('Ctrl Pts',(-7.40692737461723,-41.761356449106,-20.0475673281273));
#18008=CARTESIAN_POINT('Ctrl Pts',(-7.40774302069666,-41.7605403356751,
-20.0475711163118));
#18009=CARTESIAN_POINT('Ctrl Pts',(-7.40849348843838,-41.7597892758664,
-20.0475727773389));
#18010=CARTESIAN_POINT('Ctrl Pts',(-7.4091411982522,-41.759141187524,-20.0475730516393));
#18011=CARTESIAN_POINT('Ctrl Pts',(-7.43038644694172,-41.7378835228822,
-20.0475820488475));
#18012=CARTESIAN_POINT('Ctrl Pts',(-7.45243155834306,-41.7158301684825,
-20.0462949982859));
#18013=CARTESIAN_POINT('Ctrl Pts',(-7.47514178883455,-41.6930555178392,
-20.0434630216311));
#18014=CARTESIAN_POINT('Ctrl Pts',(-7.49785201932604,-41.6702808671958,
-20.0406310449764));
#18015=CARTESIAN_POINT('Ctrl Pts',(-7.52122758417547,-41.646784426698,-20.0362536182468));
#18016=CARTESIAN_POINT('Ctrl Pts',(-7.54510514075294,-41.6226840666228,
-20.030073463483));
#18017=CARTESIAN_POINT('Ctrl Pts',(-7.5689826973304,-41.5985837065475,-20.0238933087192));
#18018=CARTESIAN_POINT('Ctrl Pts',(-7.59336244091483,-41.5738789862741,
-20.0159097323494));
#18019=CARTESIAN_POINT('Ctrl Pts',(-7.61804933726504,-41.5487382983867,
-20.005866174252));
#18020=CARTESIAN_POINT('Ctrl Pts',(-7.62745767243902,-41.5391570203356,
-20.0020385095841));
#18021=CARTESIAN_POINT('Ctrl Pts',(-7.6371299310114,-41.5292932147427,-19.9978150359171));
#18022=CARTESIAN_POINT('Ctrl Pts',(-7.64679721452351,-41.5194120988865,
-19.9932806172721));
#18023=CARTESIAN_POINT('Ctrl Pts',(-7.65640580211876,-41.5095909772525,
-19.9887737298213));
#18024=CARTESIAN_POINT('Ctrl Pts',(-7.6660093075004,-41.4997530913086,-19.9839596558412));
#18025=CARTESIAN_POINT('Ctrl Pts',(-7.67536530938891,-41.4901498665887,
-19.9789683807891));
#18026=CARTESIAN_POINT('Ctrl Pts',(-7.68129569551421,-41.4840627760434,
-19.9758046161096));
#18027=CARTESIAN_POINT('Ctrl Pts',(-7.68712709702198,-41.4780697608219,
-19.9725706227775));
#18028=CARTESIAN_POINT('Ctrl Pts',(-7.69280255820763,-41.4722321415587,
-19.9693088409143));
#18029=CARTESIAN_POINT('Ctrl Pts',(-7.72004186109628,-41.4442145630646,
-19.9536539608574));
#18030=CARTESIAN_POINT('Ctrl Pts',(-7.74610437826649,-41.4172671980039,
-19.9360018267513));
#18031=CARTESIAN_POINT('Ctrl Pts',(-7.77095651373042,-41.3915360379521,
-19.916600253824));
#18032=CARTESIAN_POINT('Ctrl Pts',(-7.79638238142,-41.3652108526606,-19.8967507794423));
#18033=CARTESIAN_POINT('Ctrl Pts',(-7.82054133380115,-41.3401586341855,
-19.8750707073972));
#18034=CARTESIAN_POINT('Ctrl Pts',(-7.84340909674202,-41.3164822526811,
-19.8518296258943));
#18035=CARTESIAN_POINT('Ctrl Pts',(-7.85637899306561,-41.3030537326189,
-19.8386479946907));
#18036=CARTESIAN_POINT('Ctrl Pts',(-7.86893375001436,-41.2900668280115,
-19.8249642427768));
#18037=CARTESIAN_POINT('Ctrl Pts',(-7.88107054947811,-41.2775330935049,
-19.8108271605079));
#18038=CARTESIAN_POINT('Ctrl Pts',(-7.89014583714544,-41.2681609977944,
-19.8002561620539));
#18039=CARTESIAN_POINT('Ctrl Pts',(-7.89898745645573,-41.259042174888,-19.7894316870022));
#18040=CARTESIAN_POINT('Ctrl Pts',(-7.90759463769082,-41.2501796687586,
-19.7783738565697));
#18041=CARTESIAN_POINT('Ctrl Pts',(-7.91189822830837,-41.2457484156939,
-19.7728449413534));
#18042=CARTESIAN_POINT('Ctrl Pts',(-7.91635177133052,-41.241168563327,-19.7669825102079));
#18043=CARTESIAN_POINT('Ctrl Pts',(-7.92063844534917,-41.2367626882505,
-19.7611973270139));
#18044=CARTESIAN_POINT('Ctrl Pts',(-7.92492511936782,-41.2323568131741,
-19.7554121438198));
#18045=CARTESIAN_POINT('Ctrl Pts',(-7.92904514464509,-41.2281247953371,
-19.7497046604214));
#18046=CARTESIAN_POINT('Ctrl Pts',(-7.93271243794148,-41.224362680723,-19.7445201065445));
#18047=CARTESIAN_POINT('Ctrl Pts',(-7.94750683115358,-41.2091857645587,
-19.7236048640247));
#18048=CARTESIAN_POINT('Ctrl Pts',(-7.96233127313597,-41.1941459052826,
-19.7008120823441));
#18049=CARTESIAN_POINT('Ctrl Pts',(-7.97694111213783,-41.1794304558619,
-19.6760414162073));
#18050=CARTESIAN_POINT('Ctrl Pts',(-7.99130363522735,-41.1649641101307,
-19.6516900688525));
#18051=CARTESIAN_POINT('Ctrl Pts',(-8.00545868758248,-41.1508114166195,
-19.6254266232702));
#18052=CARTESIAN_POINT('Ctrl Pts',(-8.01914316314706,-41.1371752343325,
-19.5971850248403));
#18053=CARTESIAN_POINT('Ctrl Pts',(-8.02796412505137,-41.1283854020948,
-19.5789805958367));
#18054=CARTESIAN_POINT('Ctrl Pts',(-8.03650349459571,-41.1198922784968,
-19.5601396063383));
#18055=CARTESIAN_POINT('Ctrl Pts',(-8.04477864253932,-41.1116665452412,
-19.5404841542451));
#18056=CARTESIAN_POINT('Ctrl Pts',(-8.05287339486533,-41.1036201303786,
-19.521257184814));
#18057=CARTESIAN_POINT('Ctrl Pts',(-8.06071552882594,-41.0958293473494,
-19.5012505179667));
#18058=CARTESIAN_POINT('Ctrl Pts',(-8.06828468947963,-41.0882967428912,
-19.4802834837703));
#18059=CARTESIAN_POINT('Ctrl Pts',(-8.07558108464161,-41.0810355865701,
-19.4600720265333));
#18060=CARTESIAN_POINT('Ctrl Pts',(-8.08262397116933,-41.0740141770325,
-19.4389677874913));
#18061=CARTESIAN_POINT('Ctrl Pts',(-8.08935827823115,-41.0672656581897,
-19.416801005416));
#18062=CARTESIAN_POINT('Ctrl Pts',(-8.09084576985912,-41.0657750274258,
-19.4119047477233));
#18063=CARTESIAN_POINT('Ctrl Pts',(-8.092318053751,-41.0642978396422,-19.4069566307951));
#18064=CARTESIAN_POINT('Ctrl Pts',(-8.09377426946536,-41.0628346783188,
-19.4019548009793));
#18065=CARTESIAN_POINT('Ctrl Pts',(-8.10165735146519,-41.0549139969409,
-19.3748778822251));
#18066=CARTESIAN_POINT('Ctrl Pts',(-8.10829650007887,-41.048062438149,-19.3489100620048));
#18067=CARTESIAN_POINT('Ctrl Pts',(-8.11393637139768,-41.0421184216066,
-19.3242165002901));
#18068=CARTESIAN_POINT('Ctrl Pts',(-8.11612329956549,-41.0398135574578,
-19.3146412737247));
#18069=CARTESIAN_POINT('Ctrl Pts',(-8.11815976025071,-41.0376451182974,
-19.3052571196084));
#18070=CARTESIAN_POINT('Ctrl Pts',(-8.12005914140593,-41.0356036616162,
-19.2960717819185));
#18071=CARTESIAN_POINT('Ctrl Pts',(-8.12345798999853,-41.0319505758999,
-19.2796350746289));
#18072=CARTESIAN_POINT('Ctrl Pts',(-8.12641822893859,-41.0287040152778,
-19.263835506486));
#18073=CARTESIAN_POINT('Ctrl Pts',(-8.12901222214599,-41.0258106568998,
-19.2487099851899));
#18074=CARTESIAN_POINT('Ctrl Pts',(-8.13030921874969,-41.0243639777107,
-19.2411472245419));
#18075=CARTESIAN_POINT('Ctrl Pts',(-8.13151454444533,-41.0230055973182,
-19.2337529579691));
#18076=CARTESIAN_POINT('Ctrl Pts',(-8.13263671889179,-41.0217290413801,
-19.2265308114904));
#18077=CARTESIAN_POINT('Ctrl Pts',(-8.13333422540494,-41.0209355764389,
-19.2220417641558));
#18078=CARTESIAN_POINT('Ctrl Pts',(-8.13392356800037,-41.0202614215306,
-19.2181274901863));
#18079=CARTESIAN_POINT('Ctrl Pts',(-8.13455042724244,-41.0195394890359,
-19.213841617424));
#18080=CARTESIAN_POINT('Ctrl Pts',(-8.13493208248694,-41.0190999496557,
-19.2112322185235));
#18081=CARTESIAN_POINT('Ctrl Pts',(-8.13532707897324,-41.0186432748618,
-19.2084849018829));
#18082=CARTESIAN_POINT('Ctrl Pts',(-8.13576185202539,-41.0181384289453,
-19.205384314059));
#18083=CARTESIAN_POINT('Ctrl Pts',(-8.13771262528723,-41.0158732473514,
-19.191472357481));
#18084=CARTESIAN_POINT('Ctrl Pts',(-8.1395157048406,-41.0137373238154,-19.1771172970035));
#18085=CARTESIAN_POINT('Ctrl Pts',(-8.14111154314203,-41.0118111964496,
-19.1626249105981));
#18086=CARTESIAN_POINT('Ctrl Pts',(-8.1426914155545,-41.009904339417,-19.1482775162208));
#18087=CARTESIAN_POINT('Ctrl Pts',(-8.14406813862452,-41.0082032705474,
-19.1337958275692));
#18088=CARTESIAN_POINT('Ctrl Pts',(-8.14521825670048,-41.0067485722023,
-19.1194856543808));
#18089=CARTESIAN_POINT('Ctrl Pts',(-8.14564315329892,-41.0062111522699,
-19.1141989416181));
#18090=CARTESIAN_POINT('Ctrl Pts',(-8.14603746204511,-41.0057069760317,
-19.1089357048896));
#18091=CARTESIAN_POINT('Ctrl Pts',(-8.1464011799049,-41.0052367471062,-19.1037115483395));
#18092=CARTESIAN_POINT('Ctrl Pts',(-8.14714211371262,-41.0042788383895,
-19.0930693593443));
#18093=CARTESIAN_POINT('Ctrl Pts',(-8.14778974326321,-41.0034179943571,
-19.0820686180879));
#18094=CARTESIAN_POINT('Ctrl Pts',(-8.14831145781078,-41.0027000321074,
-19.0711019354135));
#18095=CARTESIAN_POINT('Ctrl Pts',(-8.14861452860038,-41.0022829584664,
-19.0647312463215));
#18096=CARTESIAN_POINT('Ctrl Pts',(-8.14887574202692,-41.0019133796073,
-19.058372166662));
#18097=CARTESIAN_POINT('Ctrl Pts',(-8.14909399641365,-41.0015941473328,
-19.052102289881));
#18098=CARTESIAN_POINT('Ctrl Pts',(-8.14936917840194,-41.0011916492509,
-19.0441970322375));
#18099=CARTESIAN_POINT('Ctrl Pts',(-8.14958925209284,-41.0008492385839,
-19.0359887114371));
#18100=CARTESIAN_POINT('Ctrl Pts',(-8.14973844015323,-41.0005922696627,
-19.0280046486033));
#18101=CARTESIAN_POINT('Ctrl Pts',(-8.14975025877486,-41.0005719126821,
-19.0273721541701));
#18102=CARTESIAN_POINT('Ctrl Pts',(-8.14976165011097,-41.0005520711957,
-19.0267410682369));
#18103=CARTESIAN_POINT('Ctrl Pts',(-8.14977261534365,-41.0005327471464,
-19.0261116534473));
#18104=CARTESIAN_POINT('Ctrl Pts',(-8.14980996055586,-41.0004669336114,
-19.023968002731));
#18105=CARTESIAN_POINT('Ctrl Pts',(-8.1498429625613,-41.0004060672224,-19.0218094180695));
#18106=CARTESIAN_POINT('Ctrl Pts',(-8.14987143029062,-41.0003504008284,
-19.0196359317889));
#18107=CARTESIAN_POINT('Ctrl Pts',(-8.149891356706,-41.0003114362984,-19.0181145673715));
#18108=CARTESIAN_POINT('Ctrl Pts',(-8.14989724819467,-41.0002995825442,
-19.017630865736));
#18109=CARTESIAN_POINT('Ctrl Pts',(-8.14991474203512,-41.0002622818322,
-19.0159905545236));
#18110=CARTESIAN_POINT('Ctrl Pts',(-8.1499222406434,-41.0002462931515,-19.0152874469765));
#18111=CARTESIAN_POINT('Ctrl Pts',(-8.14993169617691,-41.0002258364128,
-19.014371822654));
#18112=CARTESIAN_POINT('Ctrl Pts',(-8.14994303704496,-41.0001992580938,
-19.0130708039747));
#18113=CARTESIAN_POINT('Ctrl Pts',(-8.14998138787466,-41.0001093795607,
-19.0086712160803));
#18114=CARTESIAN_POINT('Ctrl Pts',(-8.14999191533451,-41.0000539914869,
-19.0053844413071));
#18115=CARTESIAN_POINT('Ctrl Pts',(-8.14999657108114,-41.0000280644039,
-19.0032071727755));
#18116=CARTESIAN_POINT('Ctrl Pts',(-8.15000109272075,-41.0000028841407,
-19.0010926196445));
#18117=CARTESIAN_POINT('Ctrl Pts',(-8.15,-41.0000001237227,-19.0000246345903));
#18118=CARTESIAN_POINT('Ctrl Pts',(-8.15,-41.,-19.));
#18119=CARTESIAN_POINT('Origin',(6.65000000000001,-41.,-19.));
#18120=CARTESIAN_POINT('Ctrl Pts',(8.15,-41.,-19.));
#18121=CARTESIAN_POINT('Ctrl Pts',(8.15,-41.0002683704757,-19.0070720744224));
#18122=CARTESIAN_POINT('Ctrl Pts',(8.15089521197314,-41.0008162323464,-19.0450824564593));
#18123=CARTESIAN_POINT('Ctrl Pts',(8.14310178514989,-41.0110134479911,-19.1473283611714));
#18124=CARTESIAN_POINT('Ctrl Pts',(8.13880142380088,-41.0161476273552,-19.188930185515));
#18125=CARTESIAN_POINT('Ctrl Pts',(8.12693222592505,-41.0289667632545,-19.2616359813663));
#18126=CARTESIAN_POINT('Ctrl Pts',(8.12206224129179,-41.0341016700959,-19.2875788667459));
#18127=CARTESIAN_POINT('Ctrl Pts',(8.1129416839662,-41.0434746813198,-19.3288153343187));
#18128=CARTESIAN_POINT('Ctrl Pts',(8.10792666252564,-41.0485793738028,-19.3500126256123));
#18129=CARTESIAN_POINT('Ctrl Pts',(8.10117431736145,-41.0553534003873,-19.3756863418201));
#18130=CARTESIAN_POINT('Ctrl Pts',(8.09807548032772,-41.0584413889392,-19.3868828152105));
#18131=CARTESIAN_POINT('Ctrl Pts',(8.09596271791297,-41.0605421677138,-19.3943891095187));
#18132=CARTESIAN_POINT('Ctrl Pts',(8.09440408811516,-41.0620877097325,-19.3998091262296));
#18133=CARTESIAN_POINT('Ctrl Pts',(8.07377569063469,-41.0825127044705,-19.470717216128));
#18134=CARTESIAN_POINT('Ctrl Pts',(8.04936906368569,-41.1063530633271,-19.5340649360603));
#18135=CARTESIAN_POINT('Ctrl Pts',(8.00832701954771,-41.146828527008,-19.6201464490146));
#18136=CARTESIAN_POINT('Ctrl Pts',(7.99390564020552,-41.1611049532053,-19.6473572700006));
#18137=CARTESIAN_POINT('Ctrl Pts',(7.96391537629543,-41.1909975275679,-19.6987524161986));
#18138=CARTESIAN_POINT('Ctrl Pts',(7.94763577235608,-41.2073325510938,-19.7239445600917));
#18139=CARTESIAN_POINT('Ctrl Pts',(7.90180834138563,-41.2536918915203,-19.7889111120554));
#18140=CARTESIAN_POINT('Ctrl Pts',(7.86689741505336,-41.2896437989342,-19.8306766770476));
#18141=CARTESIAN_POINT('Ctrl Pts',(7.80717671830243,-41.3517717037839,-19.8879120782711));
#18142=CARTESIAN_POINT('Ctrl Pts',(7.78604578677822,-41.3738393322969,-19.9060806952984));
#18143=CARTESIAN_POINT('Ctrl Pts',(7.74122618271941,-41.4206695624837,-19.9400003403023));
#18144=CARTESIAN_POINT('Ctrl Pts',(7.71886496684154,-41.4440503251323,-19.9549959652906));
#18145=CARTESIAN_POINT('Ctrl Pts',(7.63984928743279,-41.5263333775036,-19.9999263838627));
#18146=CARTESIAN_POINT('Ctrl Pts',(7.58848295448559,-41.5789080829667,-20.0192563634084));
#18147=CARTESIAN_POINT('Ctrl Pts',(7.51673107086387,-41.6514471381893,-20.0371046073696));
#18148=CARTESIAN_POINT('Ctrl Pts',(7.49368269483908,-41.674597899477,-20.0411970669247));
#18149=CARTESIAN_POINT('Ctrl Pts',(7.46071601075377,-41.7076076831635,-20.0451193489578));
#18150=CARTESIAN_POINT('Ctrl Pts',(7.44463305263381,-41.7236851791591,-20.0465257906142));
#18151=CARTESIAN_POINT('Ctrl Pts',(7.42662569081657,-41.7416724003666,-20.0473128143695));
#18152=CARTESIAN_POINT('Ctrl Pts',(7.41907557426793,-41.7492147607402,-20.0474791032032));
#18153=CARTESIAN_POINT('Ctrl Pts',(7.41407992108659,-41.7542058652218,-20.0475532708895));
#18154=CARTESIAN_POINT('Ctrl Pts',(7.41256983645835,-41.7557145519462,-20.0475716004366));
#18155=CARTESIAN_POINT('Ctrl Pts',(7.29942442170989,-41.86879388002,-20.0476194900838));
#18156=CARTESIAN_POINT('Ctrl Pts',(7.19581712569751,-41.9707644713628,-20.0142261657756));
#18157=CARTESIAN_POINT('Ctrl Pts',(7.05985359017351,-42.1031060930873,-19.9326926928216));
#18158=CARTESIAN_POINT('Ctrl Pts',(7.01768638274607,-42.1439053577669,-19.9002696352458));
#18159=CARTESIAN_POINT('Ctrl Pts',(6.95981692261362,-42.1998618651349,-19.8458099780624));
#18160=CARTESIAN_POINT('Ctrl Pts',(6.94142040681827,-42.2176450616935,-19.8266825482702));
#18161=CARTESIAN_POINT('Ctrl Pts',(6.91521906794671,-42.2430175435688,-19.7967518928284));
#18162=CARTESIAN_POINT('Ctrl Pts',(6.90671735831938,-42.2512581854557,-19.7865681729846));
#18163=CARTESIAN_POINT('Ctrl Pts',(6.89018513444049,-42.2673080364089,-19.765820985304));
#18164=CARTESIAN_POINT('Ctrl Pts',(6.88297613066536,-42.2743164823635,-19.7563895776994));
#18165=CARTESIAN_POINT('Ctrl Pts',(6.83990888094453,-42.3162962602546,-19.6970422219251));
#18166=CARTESIAN_POINT('Ctrl Pts',(6.80913262857571,-42.3469593113872,-19.6442998690234));
#18167=CARTESIAN_POINT('Ctrl Pts',(6.76870183396352,-42.3875766182603,-19.5583253785916));
#18168=CARTESIAN_POINT('Ctrl Pts',(6.75617870942774,-42.4002185564266,-19.5285226500173));
#18169=CARTESIAN_POINT('Ctrl Pts',(6.73305905770577,-42.4235267889677,-19.4667920197505));
#18170=CARTESIAN_POINT('Ctrl Pts',(6.72297996471863,-42.4336781543738,-19.436632917398));
#18171=CARTESIAN_POINT('Ctrl Pts',(6.67225353272374,-42.4841587298309,-19.2632423353073));
#18172=CARTESIAN_POINT('Ctrl Pts',(6.65128524878669,-42.5,-19.1269410506644));
#18173=CARTESIAN_POINT('Ctrl Pts',(6.65,-42.5000000000004,-19.));
#18174=CARTESIAN_POINT('Origin',(13.,-34.65,-19.));
#18175=CARTESIAN_POINT('Ctrl Pts',(14.5000000000002,-34.65,-19.));
#18176=CARTESIAN_POINT('Ctrl Pts',(14.5,-34.6502683704737,-19.0070720743719));
#18177=CARTESIAN_POINT('Ctrl Pts',(14.5008952119754,-34.6508162323428,-19.0450824563835));
#18178=CARTESIAN_POINT('Ctrl Pts',(14.4931017851574,-34.6610134479854,-19.1473283610961));
#18179=CARTESIAN_POINT('Ctrl Pts',(14.4888014238101,-34.666147627349,-19.1889301854463));
#18180=CARTESIAN_POINT('Ctrl Pts',(14.4769322259341,-34.6789667632491,-19.2616359813167));
#18181=CARTESIAN_POINT('Ctrl Pts',(14.4720622413002,-34.684101670091,-19.2875788667042));
#18182=CARTESIAN_POINT('Ctrl Pts',(14.4629416839726,-34.6934746813162,-19.328815334291));
#18183=CARTESIAN_POINT('Ctrl Pts',(14.4579266625307,-34.6985793738,-19.3500126255922));
#18184=CARTESIAN_POINT('Ctrl Pts',(14.4511743173642,-34.7053534003858,-19.3756863418097));
#18185=CARTESIAN_POINT('Ctrl Pts',(14.4480754803294,-34.7084413889382,-19.3868828152043));
#18186=CARTESIAN_POINT('Ctrl Pts',(14.4459627179139,-34.7105421677132,-19.3943891095155));
#18187=CARTESIAN_POINT('Ctrl Pts',(14.4444040881144,-34.7120877097334,-19.3998091262323));
#18188=CARTESIAN_POINT('Ctrl Pts',(14.4237756906626,-34.7325127044393,-19.4707172160325));
#18189=CARTESIAN_POINT('Ctrl Pts',(14.3993690637418,-34.7563530632669,-19.5340649359253));
#18190=CARTESIAN_POINT('Ctrl Pts',(14.3583270196135,-34.7968285269389,-19.6201464488869));
#18191=CARTESIAN_POINT('Ctrl Pts',(14.3439056402692,-34.8111049531388,-19.6473572698862));
#18192=CARTESIAN_POINT('Ctrl Pts',(14.3139153763399,-34.8409975275222,-19.6987524161288));
#18193=CARTESIAN_POINT('Ctrl Pts',(14.2976357723551,-34.8573325510948,-19.7239445600931));
#18194=CARTESIAN_POINT('Ctrl Pts',(14.2518083413899,-34.9036918915172,-19.7889111120491));
#18195=CARTESIAN_POINT('Ctrl Pts',(14.2168974150601,-34.9396437989292,-19.8306766770395));
#18196=CARTESIAN_POINT('Ctrl Pts',(14.1571767183094,-35.0017717037788,-19.887912078264));
#18197=CARTESIAN_POINT('Ctrl Pts',(14.1360457867847,-35.0238393322921,-19.9060806952923));
#18198=CARTESIAN_POINT('Ctrl Pts',(14.0912261827236,-35.0706695624807,-19.9400003402989));
#18199=CARTESIAN_POINT('Ctrl Pts',(14.0688649668324,-35.0940503251426,-19.9549959652954));
#18200=CARTESIAN_POINT('Ctrl Pts',(13.9898492874502,-35.1763333774833,-19.9999263838538));
#18201=CARTESIAN_POINT('Ctrl Pts',(13.9384829545141,-35.2289080829351,-20.0192563634001));
#18202=CARTESIAN_POINT('Ctrl Pts',(13.8667310708931,-35.3014471381576,-20.0371046073651));
#18203=CARTESIAN_POINT('Ctrl Pts',(13.8436826948659,-35.324597899448,-20.0411970669219));
#18204=CARTESIAN_POINT('Ctrl Pts',(13.8107160107728,-35.3576076831428,-20.0451193489571));
#18205=CARTESIAN_POINT('Ctrl Pts',(13.7946330526479,-35.3736851791435,-20.0465257906145));
#18206=CARTESIAN_POINT('Ctrl Pts',(13.776625690823,-35.3916724003586,-20.0473128143704));
#18207=CARTESIAN_POINT('Ctrl Pts',(13.7690755742706,-35.399214760736,-20.0474791032043));
#18208=CARTESIAN_POINT('Ctrl Pts',(13.7640799210867,-35.40420586522,-20.0475532708907));
#18209=CARTESIAN_POINT('Ctrl Pts',(13.7625698364557,-35.4057145519471,-20.0475716004378));
#18210=CARTESIAN_POINT('Ctrl Pts',(13.6494244217085,-35.5187938800181,-20.0476194900858));
#18211=CARTESIAN_POINT('Ctrl Pts',(13.5458171256972,-35.6207644713594,-20.0142261657789));
#18212=CARTESIAN_POINT('Ctrl Pts',(13.4098535901744,-35.7531060930839,-19.9326926928252));
#18213=CARTESIAN_POINT('Ctrl Pts',(13.3676863827473,-35.7939053577639,-19.9002696352492));
#18214=CARTESIAN_POINT('Ctrl Pts',(13.3098169226151,-35.8498618651327,-19.8458099780649));
#18215=CARTESIAN_POINT('Ctrl Pts',(13.2914204068199,-35.8676450616917,-19.8266825482724));
#18216=CARTESIAN_POINT('Ctrl Pts',(13.2652190679484,-35.8930175435675,-19.7967518928298));
#18217=CARTESIAN_POINT('Ctrl Pts',(13.2567173583211,-35.9012581854546,-19.7865681729857));
#18218=CARTESIAN_POINT('Ctrl Pts',(13.2401851344423,-35.9173080364082,-19.7658209853045));
#18219=CARTESIAN_POINT('Ctrl Pts',(13.232976130669,-35.9243164823613,-19.7563895777022));
#18220=CARTESIAN_POINT('Ctrl Pts',(13.1899088809391,-35.9662962602624,-19.6970422219134));
#18221=CARTESIAN_POINT('Ctrl Pts',(13.1591326285664,-35.9969593113973,-19.6442998690046));
#18222=CARTESIAN_POINT('Ctrl Pts',(13.1187018339535,-36.037576618269,-19.5583253785721));
#18223=CARTESIAN_POINT('Ctrl Pts',(13.1061787094184,-36.050218556434,-19.5285226499992));
#18224=CARTESIAN_POINT('Ctrl Pts',(13.0830590576994,-36.0735267889718,-19.4667920197387));
#18225=CARTESIAN_POINT('Ctrl Pts',(13.0729799647175,-36.0836781543729,-19.4366329174011));
#18226=CARTESIAN_POINT('Ctrl Pts',(13.0222535327245,-36.1341587298343,-19.2632423352947));
#18227=CARTESIAN_POINT('Ctrl Pts',(13.0012852487877,-36.15,-19.1269410506513));
#18228=CARTESIAN_POINT('Ctrl Pts',(13.,-36.1500000000004,-18.9999999999985));
#18229=CARTESIAN_POINT('Origin',(13.,5.15,-19.));
#18230=CARTESIAN_POINT('Ctrl Pts',(13.,6.65000000000001,-19.));
#18231=CARTESIAN_POINT('Ctrl Pts',(13.0022571542305,6.65000000000001,-19.0595221284898));
#18232=CARTESIAN_POINT('Ctrl Pts',(13.0073599851969,6.64645638324243,-19.118370455344));
#18233=CARTESIAN_POINT('Ctrl Pts',(13.0153077826458,6.63954451909008,-19.1761328970953));
#18234=CARTESIAN_POINT('Ctrl Pts',(13.01667053524,6.6383593906485,-19.1860370142866));
#18235=CARTESIAN_POINT('Ctrl Pts',(13.0181169221604,6.63707511433721,-19.1959092263041));
#18236=CARTESIAN_POINT('Ctrl Pts',(13.0196469288946,6.63569242536674,-19.2057474553742));
#18237=CARTESIAN_POINT('Ctrl Pts',(13.0232674819402,6.632420479792,-19.2290282876918));
#18238=CARTESIAN_POINT('Ctrl Pts',(13.0272868844424,6.62863709363144,-19.2518709215669));
#18239=CARTESIAN_POINT('Ctrl Pts',(13.0317769417697,6.62432546027521,-19.274508038418));
#18240=CARTESIAN_POINT('Ctrl Pts',(13.0362317965552,6.62004763059737,-19.2969676777902));
#18241=CARTESIAN_POINT('Ctrl Pts',(13.0411499681799,6.61524965955653,-19.3192254433173));
#18242=CARTESIAN_POINT('Ctrl Pts',(13.0466012500809,6.60986557248324,-19.3414979264492));
#18243=CARTESIAN_POINT('Ctrl Pts',(13.0515189167187,6.6050085231037,-19.3615902000146));
#18244=CARTESIAN_POINT('Ctrl Pts',(13.0568704390258,6.59967389575934,-19.381694590447));
#18245=CARTESIAN_POINT('Ctrl Pts',(13.0627066489669,6.59377898516122,-19.4019578562265));
#18246=CARTESIAN_POINT('Ctrl Pts',(13.0781595750536,6.57817063339199,-19.4556102696119));
#18247=CARTESIAN_POINT('Ctrl Pts',(13.0962876948866,6.55962946619751,-19.5068516933774));
#18248=CARTESIAN_POINT('Ctrl Pts',(13.1170615404503,6.53850210855677,-19.5553003604184));
#18249=CARTESIAN_POINT('Ctrl Pts',(13.1215965043478,6.53388997240436,-19.5658767823541));
#18250=CARTESIAN_POINT('Ctrl Pts',(13.1262574478565,6.52915443880112,-19.5763200413713));
#18251=CARTESIAN_POINT('Ctrl Pts',(13.1310438700908,6.52429888492631,-19.5866260128923));
#18252=CARTESIAN_POINT('Ctrl Pts',(13.1443999464643,6.51074990299114,-19.6153838900703));
#18253=CARTESIAN_POINT('Ctrl Pts',(13.1587334900103,6.49626659873545,-19.6430731920639));
#18254=CARTESIAN_POINT('Ctrl Pts',(13.1740297517247,6.48092011894879,-19.6696008381805));
#18255=CARTESIAN_POINT('Ctrl Pts',(13.181677882582,6.47324687905545,-19.6828646612388));
#18256=CARTESIAN_POINT('Ctrl Pts',(13.1895666820834,6.46535776562609,-19.6958380292713));
#18257=CARTESIAN_POINT('Ctrl Pts',(13.1976935757572,6.45726151667853,-19.7085086993931));
#18258=CARTESIAN_POINT('Ctrl Pts',(13.2017570225941,6.45321339220475,-19.714844034454));
#18259=CARTESIAN_POINT('Ctrl Pts',(13.2058799924977,6.44911347956379,-19.7211036930418));
#18260=CARTESIAN_POINT('Ctrl Pts',(13.2100621289846,6.44496286121754,-19.7272861129114));
#18261=CARTESIAN_POINT('Ctrl Pts',(13.2129317585359,6.44211485826487,-19.7315282639777));
#18262=CARTESIAN_POINT('Ctrl Pts',(13.2161072666219,6.43897225583455,-19.736126425764));
#18263=CARTESIAN_POINT('Ctrl Pts',(13.2190161563104,6.43609115059731,-19.7402712176158));
#18264=CARTESIAN_POINT('Ctrl Pts',(13.2203466199895,6.43477339492959,-19.742166956405));
#18265=CARTESIAN_POINT('Ctrl Pts',(13.2216213369736,6.43351098490738,-19.7439683311328));
#18266=CARTESIAN_POINT('Ctrl Pts',(13.2227856645693,6.4323599620326,-19.7456000774129));
#18267=CARTESIAN_POINT('Ctrl Pts',(13.2405637498981,6.41478502611381,-19.7705151654951));
#18268=CARTESIAN_POINT('Ctrl Pts',(13.2598640476524,6.39596656457336,-19.7946098108089));
#18269=CARTESIAN_POINT('Ctrl Pts',(13.2806405457862,6.37584911506449,-19.8176397930363));
#18270=CARTESIAN_POINT('Ctrl Pts',(13.300800676252,6.35632848150411,-19.8399865544269));
#18271=CARTESIAN_POINT('Ctrl Pts',(13.3223509770039,6.33558416983796,-19.8613306716731));
#18272=CARTESIAN_POINT('Ctrl Pts',(13.3452294106298,6.31358636240038,-19.8814099110357));
#18273=CARTESIAN_POINT('Ctrl Pts',(13.368057465629,6.29163699443858,-19.901444935636));
#18274=CARTESIAN_POINT('Ctrl Pts',(13.3922081788985,6.2684389191592,-19.9202204461343));
#18275=CARTESIAN_POINT('Ctrl Pts',(13.4175949294849,6.2439937051961,-19.9374391968868));
#18276=CARTESIAN_POINT('Ctrl Pts',(13.4413843218934,6.22108660704275,-19.9535745276784));
#18277=CARTESIAN_POINT('Ctrl Pts',(13.4662591457815,6.19708414904712,-19.9683422449636));
#18278=CARTESIAN_POINT('Ctrl Pts',(13.4921236616985,6.17202121567392,-19.9814718214543));
#18279=CARTESIAN_POINT('Ctrl Pts',(13.5174413758768,6.14748813778273,-19.9943238255645));
#18280=CARTESIAN_POINT('Ctrl Pts',(13.5437075604289,6.12193859062504,-20.0056057520552));
#18281=CARTESIAN_POINT('Ctrl Pts',(13.5708063058928,6.09544309122141,-20.0150455765209));
#18282=CARTESIAN_POINT('Ctrl Pts',(13.5971431852842,6.06969249796466,-20.0242200056014));
#18283=CARTESIAN_POINT('Ctrl Pts',(13.6242665787895,6.04304818801491,-20.0316539195649));
#18284=CARTESIAN_POINT('Ctrl Pts',(13.6520430849297,6.01561501023135,-20.0370874936366));
#18285=CARTESIAN_POINT('Ctrl Pts',(13.6599625404261,6.00779344226723,-20.0386366786864));
#18286=CARTESIAN_POINT('Ctrl Pts',(13.6679349096527,5.9999080132935,-20.0400232205269));
#18287=CARTESIAN_POINT('Ctrl Pts',(13.6759566644627,5.99196180702828,-20.041241039949));
#18288=CARTESIAN_POINT('Ctrl Pts',(13.6895615020033,5.97848509926772,-20.0433064527899));
#18289=CARTESIAN_POINT('Ctrl Pts',(13.703308486912,5.96483342958172,-20.0448865414512));
#18290=CARTESIAN_POINT('Ctrl Pts',(13.7171790381725,5.95102388666013,-20.0459517007041));
#18291=CARTESIAN_POINT('Ctrl Pts',(13.7241143138028,5.94411911519934,-20.0464842803305));
#18292=CARTESIAN_POINT('Ctrl Pts',(13.7310804857763,5.93717488063765,-20.046888134473));
#18293=CARTESIAN_POINT('Ctrl Pts',(13.7380750284,5.93019360707907,-20.0471595809261));
#18294=CARTESIAN_POINT('Ctrl Pts',(13.7415722997119,5.92670297029977,-20.0472953041526));
#18295=CARTESIAN_POINT('Ctrl Pts',(13.7450766640833,5.92320307422066,-20.0473979260396));
#18296=CARTESIAN_POINT('Ctrl Pts',(13.748587800006,5.91969423218044,-20.0474669897569));
#18297=CARTESIAN_POINT('Ctrl Pts',(13.7512425760986,5.91704119049648,-20.0475192089559));
#18298=CARTESIAN_POINT('Ctrl Pts',(13.7543988140328,5.91388645851485,-20.0475555844859));
#18299=CARTESIAN_POINT('Ctrl Pts',(13.7569273746163,5.91135644910865,-20.047567328126));
#18300=CARTESIAN_POINT('Ctrl Pts',(13.7577430206958,5.91054033567769,-20.0475711163105));
#18301=CARTESIAN_POINT('Ctrl Pts',(13.7584934884376,5.90978927586902,-20.0475727773376));
#18302=CARTESIAN_POINT('Ctrl Pts',(13.7591411982514,5.90914118752659,-20.047573051638));
#18303=CARTESIAN_POINT('Ctrl Pts',(13.7804931212824,5.88777678620174,-20.047582094022));
#18304=CARTESIAN_POINT('Ctrl Pts',(13.8026529826977,5.86560865026827,-20.0462820505162));
#18305=CARTESIAN_POINT('Ctrl Pts',(13.8254839293969,5.84271240272766,-20.0434202458333));
#18306=CARTESIAN_POINT('Ctrl Pts',(13.8481437807667,5.81998773988161,-20.0405798875415));
#18307=CARTESIAN_POINT('Ctrl Pts',(13.8714648760556,5.79654539898445,-20.0362005538657));
#18308=CARTESIAN_POINT('Ctrl Pts',(13.8952849872949,5.77250254010668,-20.0300268827002));
#18309=CARTESIAN_POINT('Ctrl Pts',(13.9191050985343,5.74845968122891,-20.0238532115346));
#18310=CARTESIAN_POINT('Ctrl Pts',(13.9434244185003,5.72381586942578,-20.0158845175354));
#18311=CARTESIAN_POINT('Ctrl Pts',(13.9680493372659,5.69873829838729,-20.0058661742509));
#18312=CARTESIAN_POINT('Ctrl Pts',(13.9774576724419,5.68915702033412,-20.0020385095822));
#18313=CARTESIAN_POINT('Ctrl Pts',(13.9871299310162,5.67929321473919,-19.9978150359143));
#18314=CARTESIAN_POINT('Ctrl Pts',(13.9967972145302,5.66941209888099,-19.9932806172683));
#18315=CARTESIAN_POINT('Ctrl Pts',(14.0064058021273,5.65959097724507,-19.9887737298165));
#18316=CARTESIAN_POINT('Ctrl Pts',(14.0160093075107,5.64975309129928,-19.9839596558353));
#18317=CARTESIAN_POINT('Ctrl Pts',(14.025365309401,5.64014986657743,-19.9789683807821));
#18318=CARTESIAN_POINT('Ctrl Pts',(14.0312956955227,5.63406277603582,-19.9758046161044));
#18319=CARTESIAN_POINT('Ctrl Pts',(14.037127097027,5.62806976081782,-19.972570622774));
#18320=CARTESIAN_POINT('Ctrl Pts',(14.0428025582096,5.62223214155778,-19.9693088409126));
#18321=CARTESIAN_POINT('Ctrl Pts',(14.0700418610936,5.59421456306827,-19.9536539608584));
#18322=CARTESIAN_POINT('Ctrl Pts',(14.096104378259,5.5672671980123,-19.936001826756));
#18323=CARTESIAN_POINT('Ctrl Pts',(14.1209565137182,5.54153603796518,-19.9166002538334));
#18324=CARTESIAN_POINT('Ctrl Pts',(14.1463823814028,5.51521085267855,-19.8967507794566));
#18325=CARTESIAN_POINT('Ctrl Pts',(14.170541333779,5.49015863420826,-19.8750707074175));
#18326=CARTESIAN_POINT('Ctrl Pts',(14.1934090967151,5.46648225270853,-19.8518296259219));
#18327=CARTESIAN_POINT('Ctrl Pts',(14.2063789930497,5.45305373263471,-19.8386479947084));
#18328=CARTESIAN_POINT('Ctrl Pts',(14.2189337500087,5.44006682801658,-19.8249642427839));
#18329=CARTESIAN_POINT('Ctrl Pts',(14.2310705494818,5.42753309350011,-19.8108271605039));
#18330=CARTESIAN_POINT('Ctrl Pts',(14.2401458371487,5.41816099778997,-19.8002561620504));
#18331=CARTESIAN_POINT('Ctrl Pts',(14.2489874564584,5.40904217488394,-19.7894316869992));
#18332=CARTESIAN_POINT('Ctrl Pts',(14.257594637693,5.40017966875506,-19.7783738565673));
#18333=CARTESIAN_POINT('Ctrl Pts',(14.2618982283102,5.39574841569061,-19.7728449413514));
#18334=CARTESIAN_POINT('Ctrl Pts',(14.266351771335,5.39116856332107,-19.7669825102024));
#18335=CARTESIAN_POINT('Ctrl Pts',(14.2706384453547,5.38676268824343,-19.7611973270068));
#18336=CARTESIAN_POINT('Ctrl Pts',(14.2749251193744,5.3823568131658,-19.7554121438113));
#18337=CARTESIAN_POINT('Ctrl Pts',(14.2790451446513,5.37812479532921,-19.7497046604132));
#18338=CARTESIAN_POINT('Ctrl Pts',(14.2827124379418,5.37436268072119,-19.7445201065446));
#18339=CARTESIAN_POINT('Ctrl Pts',(14.2975068310896,5.35918576462267,-19.7236048641156));
#18340=CARTESIAN_POINT('Ctrl Pts',(14.3123312730158,5.34414590540356,-19.7008120825301));
#18341=CARTESIAN_POINT('Ctrl Pts',(14.3269411119702,5.32943045603072,-19.6760414164915));
#18342=CARTESIAN_POINT('Ctrl Pts',(14.3413036350922,5.31496411026688,-19.651690069099));
#18343=CARTESIAN_POINT('Ctrl Pts',(14.355458687486,5.30081141671765,-19.6254266234608));
#18344=CARTESIAN_POINT('Ctrl Pts',(14.3691431630914,5.28717523439047,-19.5971850249547));
#18345=CARTESIAN_POINT('Ctrl Pts',(14.3779641248736,5.27838540227468,-19.5789805962081));
#18346=CARTESIAN_POINT('Ctrl Pts',(14.3865034943007,5.26989227879306,-19.5601396069914));
#18347=CARTESIAN_POINT('Ctrl Pts',(14.3947786421362,5.26166654564463,-19.5404841552019));
#18348=CARTESIAN_POINT('Ctrl Pts',(14.4028733943578,5.25362013088561,-19.521257186065));
#18349=CARTESIAN_POINT('Ctrl Pts',(14.4107155282228,5.24582934795134,-19.5012505195327));
#18350=CARTESIAN_POINT('Ctrl Pts',(14.418284688794,5.23829674357582,-19.4802834856691));
#18351=CARTESIAN_POINT('Ctrl Pts',(14.4255810838726,5.23103558733821,-19.4600720287635));
#18352=CARTESIAN_POINT('Ctrl Pts',(14.4326239703295,5.22401417787251,-19.4389677900705));
#18353=CARTESIAN_POINT('Ctrl Pts',(14.4393582773371,5.2172656590867,-19.4168010083586));
#18354=CARTESIAN_POINT('Ctrl Pts',(14.4408457692689,5.21577502801899,-19.4119047497069));
#18355=CARTESIAN_POINT('Ctrl Pts',(14.4423180534589,5.21429783993652,-19.4069566317984));
#18356=CARTESIAN_POINT('Ctrl Pts',(14.4437742694652,5.21283467831966,-19.4019548009798));
#18357=CARTESIAN_POINT('Ctrl Pts',(14.4516573514295,5.20491399697665,-19.3748778823479));
#18358=CARTESIAN_POINT('Ctrl Pts',(14.4582965000137,5.198062438216,-19.3489100622576));
#18359=CARTESIAN_POINT('Ctrl Pts',(14.4639363713086,5.19211842170032,-19.32421650068));
#18360=CARTESIAN_POINT('Ctrl Pts',(14.4661232995233,5.18981355750282,-19.3146412739223));
#18361=CARTESIAN_POINT('Ctrl Pts',(14.4681597602484,5.18764511830001,-19.3052571196246));
#18362=CARTESIAN_POINT('Ctrl Pts',(14.4700591414377,5.185603661582,-19.2960717817647));
#18363=CARTESIAN_POINT('Ctrl Pts',(14.4734579900285,5.1819505758674,-19.2796350744744));
#18364=CARTESIAN_POINT('Ctrl Pts',(14.4764182289643,5.1787040152497,-19.2638355063437));
#18365=CARTESIAN_POINT('Ctrl Pts',(14.479012222166,5.17581065687768,-19.2487099850732));
#18366=CARTESIAN_POINT('Ctrl Pts',(14.4803092187669,5.17436397769167,-19.241147224438));
#18367=CARTESIAN_POINT('Ctrl Pts',(14.4815145444593,5.17300559730254,-19.2337529578813));
#18368=CARTESIAN_POINT('Ctrl Pts',(14.4826367189024,5.17172904136818,-19.226530811422));
#18369=CARTESIAN_POINT('Ctrl Pts',(14.4833342253862,5.17093557646023,-19.2220417642747));
#18370=CARTESIAN_POINT('Ctrl Pts',(14.4839235679489,5.17026142158958,-19.2181274905262));
#18371=CARTESIAN_POINT('Ctrl Pts',(14.4845504271603,5.16953948913056,-19.2138416179853));
#18372=CARTESIAN_POINT('Ctrl Pts',(14.4849320824255,5.16909994972671,-19.2112322189507));
#18373=CARTESIAN_POINT('Ctrl Pts',(14.4853270789361,5.16864327490485,-19.2084849021477));
#18374=CARTESIAN_POINT('Ctrl Pts',(14.4857618520254,5.16813842894516,-19.2053843140591));
#18375=CARTESIAN_POINT('Ctrl Pts',(14.4877126281297,5.16587324405032,-19.19147233721));
#18376=CARTESIAN_POINT('Ctrl Pts',(14.4895157098943,5.16373731783201,-19.1771172566613));
#18377=CARTESIAN_POINT('Ctrl Pts',(14.4911115498147,5.16181118840159,-19.1626248500009));
#18378=CARTESIAN_POINT('Ctrl Pts',(14.4926914237591,5.15990432941029,-19.1482774362137));
#18379=CARTESIAN_POINT('Ctrl Pts',(14.4940681477991,5.15820325916898,-19.1337957279846));
#18380=CARTESIAN_POINT('Ctrl Pts',(14.495218266324,5.15674856003158,-19.119485534642));
#18381=CARTESIAN_POINT('Ctrl Pts',(14.4956431592295,5.1562111446872,-19.1141988624459));
#18382=CARTESIAN_POINT('Ctrl Pts',(14.4960374647681,5.15570697251119,-19.1089356657791));
#18383=CARTESIAN_POINT('Ctrl Pts',(14.4964011799049,5.15523674710575,-19.1037115483395));
#18384=CARTESIAN_POINT('Ctrl Pts',(14.4971421224544,5.1542788270869,-19.093069233785));
#18385=CARTESIAN_POINT('Ctrl Pts',(14.4977897578427,5.15341797497385,-19.0820683695518));
#18386=CARTESIAN_POINT('Ctrl Pts',(14.4983114755707,5.15270000767031,-19.0711015620904));
#18387=CARTESIAN_POINT('Ctrl Pts',(14.4986145386453,5.15228294425303,-19.0647310015177));
#18388=CARTESIAN_POINT('Ctrl Pts',(14.4988757461215,5.1519133736185,-19.0583720490357));
#18389=CARTESIAN_POINT('Ctrl Pts',(14.4990939964136,5.15159414733242,-19.052102289881));
#18390=CARTESIAN_POINT('Ctrl Pts',(14.4993691946477,5.1511916254878,-19.0441965655395));
#18391=CARTESIAN_POINT('Ctrl Pts',(14.4995892765542,5.15084920049255,-19.0359877955948));
#18392=CARTESIAN_POINT('Ctrl Pts',(14.4997384658976,5.15059222531898,-19.0280032708125));
#18393=CARTESIAN_POINT('Ctrl Pts',(14.499750275309,5.15057188388268,-19.0273712381535));
#18394=CARTESIAN_POINT('Ctrl Pts',(14.4997616580645,5.15055205717901,-19.0267406116957));
#18395=CARTESIAN_POINT('Ctrl Pts',(14.4997726153437,5.15053274714614,-19.0261116534473));
#18396=CARTESIAN_POINT('Ctrl Pts',(14.4998099607338,5.15046693329733,-19.0239679925148));
#18397=CARTESIAN_POINT('Ctrl Pts',(14.4998429627843,5.15040606680349,-19.0218094027432));
#18398=CARTESIAN_POINT('Ctrl Pts',(14.4998714304914,5.15035040043575,-19.0196359164617));
#18399=CARTESIAN_POINT('Ctrl Pts',(14.4998913568769,5.15031143595214,-19.0181145531323));
#18400=CARTESIAN_POINT('Ctrl Pts',(14.499897248271,5.15029958238154,-19.017630858564));
#18401=CARTESIAN_POINT('Ctrl Pts',(14.4999147420333,5.1502622818361,-19.0159905546918));
#18402=CARTESIAN_POINT('Ctrl Pts',(14.499922240626,5.15024629318873,-19.0152874486141));
#18403=CARTESIAN_POINT('Ctrl Pts',(14.4999316961582,5.15022583645654,-19.0143718247977));
#18404=CARTESIAN_POINT('Ctrl Pts',(14.499943037045,5.15019925809364,-19.0130708039746));
#18405=CARTESIAN_POINT('Ctrl Pts',(14.4999813878725,5.15010937956514,-19.0086712163258));
#18406=CARTESIAN_POINT('Ctrl Pts',(14.4999919153334,5.15005399149088,-19.0053844416258));
#18407=CARTESIAN_POINT('Ctrl Pts',(14.4999965710805,5.15002806440687,-19.0032071730684));
#18408=CARTESIAN_POINT('Ctrl Pts',(14.5000010927209,5.15000288414101,-19.0010926197659));
#18409=CARTESIAN_POINT('Ctrl Pts',(14.5,5.15000012372276,-19.0000246345919));
#18410=CARTESIAN_POINT('Ctrl Pts',(14.5,5.15,-19.));
#18411=CARTESIAN_POINT('Origin',(0.,0.,-19.5));
#18412=CARTESIAN_POINT('Origin',(15.87105808376,-20.475,12.5));
#18413=CARTESIAN_POINT('',(14.4421161675142,-17.9999999999976,12.5));
#18414=CARTESIAN_POINT('Origin',(14.44211616751,-18.,12.5));
#18415=CARTESIAN_POINT('Origin',(15.87105808376,1.525,12.5));
#18416=CARTESIAN_POINT('',(14.4421161675142,4.00000000000243,12.5));
#18417=CARTESIAN_POINT('Origin',(14.44211616751,4.,12.5));
#18418=CARTESIAN_POINT('Origin',(0.,0.,-5.));
#18419=CARTESIAN_POINT('',(13.75,0.,-5.));
#18420=CARTESIAN_POINT('',(18.88,-23.05,-5.));
#18421=CARTESIAN_POINT('',(13.98,-23.05,-5.));
#18422=CARTESIAN_POINT('',(0.,-23.05,-5.));
#18423=CARTESIAN_POINT('',(18.88,-37.95,-5.));
#18424=CARTESIAN_POINT('',(18.88,0.,-5.));
#18425=CARTESIAN_POINT('',(13.98,-37.95,-5.));
#18426=CARTESIAN_POINT('',(0.,-37.95,-5.));
#18427=CARTESIAN_POINT('',(13.98,0.,-5.));
#18428=CARTESIAN_POINT('Origin',(13.75,-22.475,12.5));
#18429=CARTESIAN_POINT('Origin',(13.475,-43.87105808376,12.5));
#18430=CARTESIAN_POINT('',(13.475,-43.87105808376,12.5));
#18431=CARTESIAN_POINT('Origin',(11.,-42.44211616751,12.5));
#18432=CARTESIAN_POINT('',(11.0000000000008,-42.4421161675114,12.5));
#18433=CARTESIAN_POINT('',(11.,-42.44211616751,12.5));
#18434=CARTESIAN_POINT('',(11.,-42.44211616751,12.5));
#18435=CARTESIAN_POINT('Origin',(8.525,-43.87105808376,12.5));
#18436=CARTESIAN_POINT('',(8.525,-43.87105808376,12.5));
#18437=CARTESIAN_POINT('',(8.525,-43.87105808376,12.5));
#18438=CARTESIAN_POINT('Origin',(-11.,-42.44211616751,12.5));
#18439=CARTESIAN_POINT('',(-11.,-42.44211616751,12.5));
#18440=CARTESIAN_POINT('',(-11.,-42.44211616751,12.5));
#18441=CARTESIAN_POINT('Origin',(0.,0.,12.5));
#18442=CARTESIAN_POINT('Origin',(0.,0.,12.5));
#18443=CARTESIAN_POINT('Origin',(0.,0.,12.5));
#18444=CARTESIAN_POINT('Origin',(0.,0.,-12.5));
#18445=CARTESIAN_POINT('Origin',(0.,0.,-12.5));
#18446=CARTESIAN_POINT('Origin',(0.,0.,12.5));
#18447=CARTESIAN_POINT('Origin',(-13.98,-23.05,-5.));
#18448=CARTESIAN_POINT('',(-18.88,-23.05,-4.1));
#18449=CARTESIAN_POINT('',(-13.98,-23.05,-4.1));
#18450=CARTESIAN_POINT('',(-13.98,-23.05,-4.1));
#18451=CARTESIAN_POINT('',(-13.98,-23.05,-5.));
#18452=CARTESIAN_POINT('',(-18.88,-23.05,-5.));
#18453=CARTESIAN_POINT('Origin',(-13.98,-37.95,-5.));
#18454=CARTESIAN_POINT('',(-13.98,-37.95,-4.1));
#18455=CARTESIAN_POINT('',(-13.98,-37.95,-4.1));
#18456=CARTESIAN_POINT('',(-13.98,-37.95,-5.));
#18457=CARTESIAN_POINT('Origin',(-18.88,-37.95,-5.));
#18458=CARTESIAN_POINT('',(-18.88,-37.95,-4.1));
#18459=CARTESIAN_POINT('',(-18.88,-37.95,-4.1));
#18460=CARTESIAN_POINT('',(-18.88,-37.95,-5.));
#18461=CARTESIAN_POINT('Origin',(-18.88,-23.05,-5.));
#18462=CARTESIAN_POINT('',(-18.88,-23.05,-4.1));
#18463=CARTESIAN_POINT('Ctrl Pts',(-12.9943339616048,6.64999987669794,-18.9993941238939));
#18464=CARTESIAN_POINT('Ctrl Pts',(-13.2370215098806,6.64999993944614,-19.001183928572));
#18465=CARTESIAN_POINT('Ctrl Pts',(-13.4998389840212,6.64999999595731,-18.742870425708));
#18466=CARTESIAN_POINT('Ctrl Pts',(-13.4997146189277,6.64999995914459,-18.4999999987164));
#18467=CARTESIAN_POINT('Ctrl Pts',(-12.9952528649784,6.65005651677245,-19.1408685056908));
#18468=CARTESIAN_POINT('Ctrl Pts',(-13.2563860307187,6.65002775365178,-19.0952152758849));
#18469=CARTESIAN_POINT('Ctrl Pts',(-13.5368119433216,6.65000184997225,-18.7900242993434));
#18470=CARTESIAN_POINT('Ctrl Pts',(-13.5652595935244,6.65001872630134,-18.4999999984663));
#18471=CARTESIAN_POINT('Ctrl Pts',(-13.0396126023806,6.61116933174272,-19.4140223461765));
#18472=CARTESIAN_POINT('Ctrl Pts',(-13.3232070225677,6.63093544404987,-19.2738284330859));
#18473=CARTESIAN_POINT('Ctrl Pts',(-13.6226027377202,6.64873553214766,-18.8824627820465));
#18474=CARTESIAN_POINT('Ctrl Pts',(-13.6962559207404,6.63713438038325,-18.4999999979752));
#18475=CARTESIAN_POINT('Ctrl Pts',(-13.2092320493187,6.44517535101228,-19.7671081794715));
#18476=CARTESIAN_POINT('Ctrl Pts',(-13.4926490904923,6.5329355447166,-19.5234352013649));
#18477=CARTESIAN_POINT('Ctrl Pts',(-13.7989275084018,6.61612657000081,-18.9987393235434));
#18478=CARTESIAN_POINT('Ctrl Pts',(-13.8851496535813,6.57983328116779,-18.499999997364));
#18479=CARTESIAN_POINT('Ctrl Pts',(-13.4604801612314,6.1970778370455,-20.0000694996498));
#18480=CARTESIAN_POINT('Ctrl Pts',(-13.7204167792394,6.35869299291861,-19.700859717038));
#18481=CARTESIAN_POINT('Ctrl Pts',(-14.009795050356,6.52385442234337,-19.0757337060942));
#18482=CARTESIAN_POINT('Ctrl Pts',(-14.0591509646277,6.48682859378864,-18.4999999969598));
#18483=CARTESIAN_POINT('Ctrl Pts',(-13.7542035734046,5.90426917911432,-20.0822650788903));
#18484=CARTESIAN_POINT('Ctrl Pts',(-13.9754027621768,6.12558454016965,-19.7657545358291));
#18485=CARTESIAN_POINT('Ctrl Pts',(-14.214781365486,6.36471268348123,-19.1045289473903));
#18486=CARTESIAN_POINT('Ctrl Pts',(-14.2116652821764,6.36166528217619,-18.4999999968019));
#18487=CARTESIAN_POINT('Ctrl Pts',(-14.0470674075829,5.61021883748008,-20.0001437555208));
#18488=CARTESIAN_POINT('Ctrl Pts',(-14.209895391559,5.87040128717705,-19.6998305081928));
#18489=CARTESIAN_POINT('Ctrl Pts',(-14.3737201797862,6.15993553582587,-19.0761517589312));
#18490=CARTESIAN_POINT('Ctrl Pts',(-14.336828593787,6.20915096462532,-18.499999996955));
#18491=CARTESIAN_POINT('Ctrl Pts',(-14.2951361405339,5.36009661840369,-19.7669964902509));
#18492=CARTESIAN_POINT('Ctrl Pts',(-14.3844114694822,5.64346751311684,-19.5204897565764));
#18493=CARTESIAN_POINT('Ctrl Pts',(-14.4661360608765,5.94912088712555,-18.9989428562545));
#18494=CARTESIAN_POINT('Ctrl Pts',(-14.4298332811648,6.0351496535811,-18.4999999973626));
#18495=CARTESIAN_POINT('Ctrl Pts',(-14.4611328976568,5.18703565679378,-19.4146293224293));
#18496=CARTESIAN_POINT('Ctrl Pts',(-14.482540122838,5.47116307253208,-19.270971688124));
#18497=CARTESIAN_POINT('Ctrl Pts',(-14.4987564117522,5.77187033265161,-18.8811859318062));
#18498=CARTESIAN_POINT('Ctrl Pts',(-14.4871343803804,5.84625592074344,-18.4999999979862));
#18499=CARTESIAN_POINT('Ctrl Pts',(-14.5000565697471,5.14917290265596,-19.1402100483587));
#18500=CARTESIAN_POINT('Ctrl Pts',(-14.5000254205556,5.40884039973222,-19.088420003154));
#18501=CARTESIAN_POINT('Ctrl Pts',(-14.5000018196169,5.6881172092188,-18.7897579239478));
#18502=CARTESIAN_POINT('Ctrl Pts',(-14.5000187262999,5.71525959351538,-18.4999999984668));
#18503=CARTESIAN_POINT('Ctrl Pts',(-14.4999998765826,5.14432072445288,-18.9995579554861));
#18504=CARTESIAN_POINT('Ctrl Pts',(-14.499999944535,5.38684649954523,-18.9943613932106));
#18505=CARTESIAN_POINT('Ctrl Pts',(-14.4999999960227,5.64983329085767,-18.7428715921064));
#18506=CARTESIAN_POINT('Ctrl Pts',(-14.4999999591429,5.64971461892676,-18.4999999987146));
#18507=CARTESIAN_POINT('Ctrl Pts',(-14.5000000000013,-34.6443380969227,
-19.0000100692442));
#18508=CARTESIAN_POINT('Ctrl Pts',(-14.5000000000008,-34.8871059113903,
-19.0015933091084));
#18509=CARTESIAN_POINT('Ctrl Pts',(-14.5000000000027,-35.1500000009281,
-18.7430757267126));
#18510=CARTESIAN_POINT('Ctrl Pts',(-14.5000000000019,-35.15,-18.4999999987137));
#18511=CARTESIAN_POINT('Ctrl Pts',(-14.5000000000028,-34.645317328355,-19.1412652085388));
#18512=CARTESIAN_POINT('Ctrl Pts',(-14.5000000000014,-34.9064831044291,
-19.0954746833564));
#18513=CARTESIAN_POINT('Ctrl Pts',(-14.5000000000026,-35.1869365607809,
-18.7901585471376));
#18514=CARTESIAN_POINT('Ctrl Pts',(-14.5000000000014,-35.215449847102,-18.4999999984638));
#18515=CARTESIAN_POINT('Ctrl Pts',(-14.461088950263,-34.6896947394679,-19.4141933256417));
#18516=CARTESIAN_POINT('Ctrl Pts',(-14.4808879882492,-34.9732890737612,
-19.2739493035027));
#18517=CARTESIAN_POINT('Ctrl Pts',(-14.4987197414757,-35.272688121818,-18.8825190881865));
#18518=CARTESIAN_POINT('Ctrl Pts',(-14.4871066327079,-35.3463473912737,
-18.4999999979725));
#18519=CARTESIAN_POINT('Ctrl Pts',(-14.2951753510104,-34.8592320493177,
-19.7671081794723));
#18520=CARTESIAN_POINT('Ctrl Pts',(-14.3829355447186,-35.1426490904922,
-19.5234352013656));
#18521=CARTESIAN_POINT('Ctrl Pts',(-14.466126570005,-35.448927508403,-18.9987393235418));
#18522=CARTESIAN_POINT('Ctrl Pts',(-14.4298332811675,-35.5351496535818,
-18.4999999973609));
#18523=CARTESIAN_POINT('Ctrl Pts',(-14.0470778370451,-35.1104801612305,
-20.0000694996508));
#18524=CARTESIAN_POINT('Ctrl Pts',(-14.208692992919,-35.3704167792393,-19.7008597170388));
#18525=CARTESIAN_POINT('Ctrl Pts',(-14.373854422343,-35.6597950503571,-19.0757337060923));
#18526=CARTESIAN_POINT('Ctrl Pts',(-14.3368285937893,-35.709150964628,-18.4999999969561));
#18527=CARTESIAN_POINT('Ctrl Pts',(-13.7542691791144,-35.4042035734038,
-20.0822650788914));
#18528=CARTESIAN_POINT('Ctrl Pts',(-13.9755845401677,-35.6254027621767,
-19.7657545358299));
#18529=CARTESIAN_POINT('Ctrl Pts',(-14.2147126834794,-35.864781365487,-19.1045289473882));
#18530=CARTESIAN_POINT('Ctrl Pts',(-14.2116652821725,-35.8616652821764,
-18.4999999967981));
#18531=CARTESIAN_POINT('Ctrl Pts',(-13.4602188374819,-35.6970674075824,
-20.0001437555219));
#18532=CARTESIAN_POINT('Ctrl Pts',(-13.7204012871743,-35.859895391559,-19.6998305081936));
#18533=CARTESIAN_POINT('Ctrl Pts',(-14.0099355358227,-36.023720179787,-19.0761517589292));
#18534=CARTESIAN_POINT('Ctrl Pts',(-14.0591509646221,-35.9868285937868,
-18.4999999969514));
#18535=CARTESIAN_POINT('Ctrl Pts',(-13.2100966184005,-35.9451361405336,
-19.7669964902518));
#18536=CARTESIAN_POINT('Ctrl Pts',(-13.4934675131165,-36.0344114694822,
-19.5204897565771));
#18537=CARTESIAN_POINT('Ctrl Pts',(-13.7991208871267,-36.1161360608768,
-18.9989428562529));
#18538=CARTESIAN_POINT('Ctrl Pts',(-13.8851496535816,-36.0798332811645,
-18.4999999973594));
#18539=CARTESIAN_POINT('Ctrl Pts',(-13.0371194604123,-36.1110525148315,
-19.4147999538865));
#18540=CARTESIAN_POINT('Ctrl Pts',(-13.3212465098146,-36.1324926046905,
-19.2710925155892));
#18541=CARTESIAN_POINT('Ctrl Pts',(-13.6219561650579,-36.1487406155644,
-18.8812429548123));
#18542=CARTESIAN_POINT('Ctrl Pts',(-13.6963473912789,-36.1371066327043,
-18.4999999979835));
#18543=CARTESIAN_POINT('Ctrl Pts',(-12.9992279345901,-36.1500000000002,
-19.1406085881773));
#18544=CARTESIAN_POINT('Ctrl Pts',(-13.2589309435621,-36.1500000000008,
-19.0886851287514));
#18545=CARTESIAN_POINT('Ctrl Pts',(-13.5382388686105,-36.1499999999992,
-18.7898907052044));
#18546=CARTESIAN_POINT('Ctrl Pts',(-13.5654498470941,-36.1499999999989,
-18.4999999984642));
#18547=CARTESIAN_POINT('Ctrl Pts',(-12.9943419397749,-36.1500000000006,
-19.0001703298077));
#18548=CARTESIAN_POINT('Ctrl Pts',(-13.2369423184852,-36.1500000000009,
-18.9947709047232));
#18549=CARTESIAN_POINT('Ctrl Pts',(-13.5000000009278,-36.1499999999995,
-18.7430757267406));
#18550=CARTESIAN_POINT('Ctrl Pts',(-13.4999999999998,-36.1499999999986,
-18.499999998712));
#18551=CARTESIAN_POINT('Ctrl Pts',(-8.14999999999987,-40.9943380969236,
-19.0000100692442));
#18552=CARTESIAN_POINT('Ctrl Pts',(-8.1500000000003,-41.237105911391,-19.0015933091078));
#18553=CARTESIAN_POINT('Ctrl Pts',(-8.15000000000033,-41.5000000009281,
-18.7430757267123));
#18554=CARTESIAN_POINT('Ctrl Pts',(-8.15000000000025,-41.5,-18.4999999987137));
#18555=CARTESIAN_POINT('Ctrl Pts',(-8.15000000000028,-40.9953173283559,
-19.1412652085387));
#18556=CARTESIAN_POINT('Ctrl Pts',(-8.15000000000049,-41.2564831044297,
-19.0954746833557));
#18557=CARTESIAN_POINT('Ctrl Pts',(-8.15000000000039,-41.536936560781,-18.7901585471373));
#18558=CARTESIAN_POINT('Ctrl Pts',(-8.15000000000039,-41.565449847102,-18.4999999984638));
#18559=CARTESIAN_POINT('Ctrl Pts',(-8.11108895026239,-41.0396947394688,
-19.4141933256412));
#18560=CARTESIAN_POINT('Ctrl Pts',(-8.13088798825094,-41.3232890737619,
-19.2739493035018));
#18561=CARTESIAN_POINT('Ctrl Pts',(-8.14871974147486,-41.6226881218181,
-18.8825190881861));
#18562=CARTESIAN_POINT('Ctrl Pts',(-8.13710663270727,-41.6963473912737,
-18.4999999979725));
#18563=CARTESIAN_POINT('Ctrl Pts',(-7.94517535101228,-41.2092320493187,
-19.7671081794715));
#18564=CARTESIAN_POINT('Ctrl Pts',(-8.03293554471679,-41.4926490904929,
-19.5234352013644));
#18565=CARTESIAN_POINT('Ctrl Pts',(-8.11612657000116,-41.7989275084031,
-18.9987393235412));
#18566=CARTESIAN_POINT('Ctrl Pts',(-8.07983328116756,-41.8851496535818,
-18.4999999973609));
#18567=CARTESIAN_POINT('Ctrl Pts',(-7.69707783704551,-41.4604801612314,
-20.0000694996498));
#18568=CARTESIAN_POINT('Ctrl Pts',(-7.85869299291896,-41.72041677924,-19.7008597170374));
#18569=CARTESIAN_POINT('Ctrl Pts',(-8.02385442234407,-42.0097950503572,
-19.0757337060916));
#18570=CARTESIAN_POINT('Ctrl Pts',(-7.98682859378841,-42.059150964628,-18.4999999969561));
#18571=CARTESIAN_POINT('Ctrl Pts',(-7.40426917911432,-41.7542035734046,
-20.0822650788903));
#18572=CARTESIAN_POINT('Ctrl Pts',(-7.62558454017011,-41.9754027621772,
-19.7657545358284));
#18573=CARTESIAN_POINT('Ctrl Pts',(-7.86471268348223,-42.214781365487,-19.1045289473875));
#18574=CARTESIAN_POINT('Ctrl Pts',(-7.86166528217617,-42.2116652821764,
-18.4999999967981));
#18575=CARTESIAN_POINT('Ctrl Pts',(-7.11021883748008,-42.0470674075829,
-20.0001437555208));
#18576=CARTESIAN_POINT('Ctrl Pts',(-7.3704012871776,-42.2098953915593,-19.6998305081922));
#18577=CARTESIAN_POINT('Ctrl Pts',(-7.65993553582709,-42.3737201797869,
-19.0761517589285));
#18578=CARTESIAN_POINT('Ctrl Pts',(-7.70915096462563,-42.3368285937868,
-18.4999999969514));
#18579=CARTESIAN_POINT('Ctrl Pts',(-6.86009661840369,-42.2951361405338,
-19.7669964902509));
#18580=CARTESIAN_POINT('Ctrl Pts',(-7.14346751311743,-42.3844114694824,
-19.5204897565759));
#18581=CARTESIAN_POINT('Ctrl Pts',(-7.44912088712684,-42.4661360608768,
-18.9989428562523));
#18582=CARTESIAN_POINT('Ctrl Pts',(-7.53514965358164,-42.4298332811645,
-18.4999999973594));
#18583=CARTESIAN_POINT('Ctrl Pts',(-6.68711946041285,-42.4610525148318,
-19.4147999538856));
#18584=CARTESIAN_POINT('Ctrl Pts',(-6.97124650981146,-42.4824926046906,
-19.271092515588));
#18585=CARTESIAN_POINT('Ctrl Pts',(-7.2719561650544,-42.4987406155645,-18.8812429548117));
#18586=CARTESIAN_POINT('Ctrl Pts',(-7.34634739127708,-42.4871066327043,
-18.4999999979835));
#18587=CARTESIAN_POINT('Ctrl Pts',(-6.64922793459199,-42.5000000000004,
-19.1406085881762));
#18588=CARTESIAN_POINT('Ctrl Pts',(-6.90893094356097,-42.5000000000009,
-19.0886851287501));
#18589=CARTESIAN_POINT('Ctrl Pts',(-7.1882388686094,-42.4999999999992,-18.7898907052038));
#18590=CARTESIAN_POINT('Ctrl Pts',(-7.21544984709361,-42.4999999999989,
-18.4999999984642));
#18591=CARTESIAN_POINT('Ctrl Pts',(-6.64434193977743,-42.5000000000005,
-19.0001703298062));
#18592=CARTESIAN_POINT('Ctrl Pts',(-6.88694231848536,-42.5000000000009,
-18.9947709047217));
#18593=CARTESIAN_POINT('Ctrl Pts',(-7.15000000092837,-42.4999999999995,
-18.7430757267398));
#18594=CARTESIAN_POINT('Ctrl Pts',(-7.15,-42.4999999999986,-18.499999998712));
#18595=CARTESIAN_POINT('Ctrl Pts',(6.64433396160519,-42.499999876699,-18.9993941238985));
#18596=CARTESIAN_POINT('Ctrl Pts',(6.88702150988135,-42.4999999394466,-19.001183928576));
#18597=CARTESIAN_POINT('Ctrl Pts',(7.14983898402066,-42.4999999959597,-18.74287042571));
#18598=CARTESIAN_POINT('Ctrl Pts',(7.14971461892777,-42.4999999591463,-18.4999999987164));
#18599=CARTESIAN_POINT('Ctrl Pts',(6.6452528649791,-42.5000565167741,-19.140868505694));
#18600=CARTESIAN_POINT('Ctrl Pts',(6.90638603072031,-42.5000277536524,-19.095215275888));
#18601=CARTESIAN_POINT('Ctrl Pts',(7.1868119433205,-42.5000018499744,-18.7900242993449));
#18602=CARTESIAN_POINT('Ctrl Pts',(7.2152595935232,-42.5000187263022,-18.4999999984663));
#18603=CARTESIAN_POINT('Ctrl Pts',(6.68961260237979,-42.4611693317427,-19.4140223461786));
#18604=CARTESIAN_POINT('Ctrl Pts',(6.97320702256912,-42.4809354440478,-19.2738284330882));
#18605=CARTESIAN_POINT('Ctrl Pts',(7.27260273771983,-42.4987355321484,-18.8824627820476));
#18606=CARTESIAN_POINT('Ctrl Pts',(7.34625592074007,-42.4871343803837,-18.4999999979752));
#18607=CARTESIAN_POINT('Ctrl Pts',(6.85923204931696,-42.2951753510103,-19.7671081794728));
#18608=CARTESIAN_POINT('Ctrl Pts',(7.14264909049096,-42.3829355447183,-19.5234352013668));
#18609=CARTESIAN_POINT('Ctrl Pts',(7.44892750840371,-42.4661265700047,-18.9987393235443));
#18610=CARTESIAN_POINT('Ctrl Pts',(7.53514965358202,-42.4298332811677,-18.499999997364));
#18611=CARTESIAN_POINT('Ctrl Pts',(7.11048016122898,-42.0470778370448,-20.0000694996515));
#18612=CARTESIAN_POINT('Ctrl Pts',(7.37041677923766,-42.2086929929184,-19.7008597170403));
#18613=CARTESIAN_POINT('Ctrl Pts',(7.65979505035629,-42.3738544223423,-19.0757337060953));
#18614=CARTESIAN_POINT('Ctrl Pts',(7.70915096462646,-42.3368285937896,-18.4999999969597));
#18615=CARTESIAN_POINT('Ctrl Pts',(7.4042035734027,-41.754269179114,-20.0822650788921));
#18616=CARTESIAN_POINT('Ctrl Pts',(7.62540276217399,-41.9755845401669,-19.7657545358315));
#18617=CARTESIAN_POINT('Ctrl Pts',(7.86478136548691,-42.2147126834784,-19.1045289473914));
#18618=CARTESIAN_POINT('Ctrl Pts',(7.86166528217616,-42.2116652821725,-18.4999999968019));
#18619=CARTESIAN_POINT('Ctrl Pts',(7.69706740757966,-41.4602188374814,-20.0001437555225));
#18620=CARTESIAN_POINT('Ctrl Pts',(7.85989539155775,-41.7204012871734,-19.6998305081951));
#18621=CARTESIAN_POINT('Ctrl Pts',(8.02372017978781,-42.0099355358214,-19.0761517589322));
#18622=CARTESIAN_POINT('Ctrl Pts',(7.98682859378959,-42.0591509646218,-18.499999996955));
#18623=CARTESIAN_POINT('Ctrl Pts',(7.94513614053531,-41.2100966184,-19.7669964902523));
#18624=CARTESIAN_POINT('Ctrl Pts',(8.0344114694836,-41.4934675131155,-19.5204897565783));
#18625=CARTESIAN_POINT('Ctrl Pts',(8.11613606087722,-41.7991208871254,-18.9989428562554));
#18626=CARTESIAN_POINT('Ctrl Pts',(8.07983328116767,-41.8851496535811,-18.4999999973625));
#18627=CARTESIAN_POINT('Ctrl Pts',(8.11113289765597,-41.037035656793,-19.4146293224311));
#18628=CARTESIAN_POINT('Ctrl Pts',(8.13254012283828,-41.3211630725351,-19.2709716881261));
#18629=CARTESIAN_POINT('Ctrl Pts',(8.14875641175435,-41.6218703326553,-18.8811859318073));
#18630=CARTESIAN_POINT('Ctrl Pts',(8.13713438038314,-41.6962559207456,-18.4999999979862));
#18631=CARTESIAN_POINT('Ctrl Pts',(8.15005656974628,-40.9991729026537,-19.1402100483613));
#18632=CARTESIAN_POINT('Ctrl Pts',(8.15002542055481,-41.2588403997333,-19.0884200031566));
#18633=CARTESIAN_POINT('Ctrl Pts',(8.15000181961798,-41.5381172092203,-18.7897579239491));
#18634=CARTESIAN_POINT('Ctrl Pts',(8.15001872630097,-41.5652595935165,-18.4999999984667));
#18635=CARTESIAN_POINT('Ctrl Pts',(8.14999987658211,-40.9943207244499,-18.9995579554898));
#18636=CARTESIAN_POINT('Ctrl Pts',(8.14999994453439,-41.2368464995451,-18.994361393214));
#18637=CARTESIAN_POINT('Ctrl Pts',(8.14999999602334,-41.4998332908577,-18.742871592108));
#18638=CARTESIAN_POINT('Ctrl Pts',(8.14999995914438,-41.4997146189276,-18.4999999987146));
#18639=CARTESIAN_POINT('Ctrl Pts',(12.9943339616049,-36.149999876699,-18.9993941238957));
#18640=CARTESIAN_POINT('Ctrl Pts',(13.2370215098809,-36.1499999394466,-19.001183928573));
#18641=CARTESIAN_POINT('Ctrl Pts',(13.4998389840216,-36.1499999959597,-18.7428704257086));
#18642=CARTESIAN_POINT('Ctrl Pts',(13.4997146189285,-36.1499999591463,-18.4999999987164));
#18643=CARTESIAN_POINT('Ctrl Pts',(12.9952528649788,-36.1500565167744,-19.1408685056919));
#18644=CARTESIAN_POINT('Ctrl Pts',(13.2563860307191,-36.1500277536526,-19.0952152758855));
#18645=CARTESIAN_POINT('Ctrl Pts',(13.536811943322,-36.1500018499744,-18.7900242993437));
#18646=CARTESIAN_POINT('Ctrl Pts',(13.5652595935249,-36.1500187263023,-18.4999999984663));
#18647=CARTESIAN_POINT('Ctrl Pts',(13.039612602381,-36.1111693317432,-19.4140223461769));
#18648=CARTESIAN_POINT('Ctrl Pts',(13.3232070225681,-36.1309354440481,-19.2738284330861));
#18649=CARTESIAN_POINT('Ctrl Pts',(13.6226027377205,-36.1487355321485,-18.8824627820465));
#18650=CARTESIAN_POINT('Ctrl Pts',(13.6962559207406,-36.1371343803838,-18.4999999979752));
#18651=CARTESIAN_POINT('Ctrl Pts',(13.2092320493188,-35.9451753510108,-19.7671081794713));
#18652=CARTESIAN_POINT('Ctrl Pts',(13.4926490904924,-36.0329355447186,-19.5234352013647));
#18653=CARTESIAN_POINT('Ctrl Pts',(13.7989275084019,-36.1161265700046,-18.9987393235433));
#18654=CARTESIAN_POINT('Ctrl Pts',(13.8851496535813,-36.0798332811677,-18.499999997364));
#18655=CARTESIAN_POINT('Ctrl Pts',(13.4604801612315,-35.6970778370458,-20.0000694996497));
#18656=CARTESIAN_POINT('Ctrl Pts',(13.7204167792395,-35.8586929929191,-19.7008597170378));
#18657=CARTESIAN_POINT('Ctrl Pts',(14.009795050356,-36.0238544223422,-19.0757337060941));
#18658=CARTESIAN_POINT('Ctrl Pts',(14.0591509646277,-35.9868285937896,-18.4999999969598));
#18659=CARTESIAN_POINT('Ctrl Pts',(13.7542035734047,-35.4042691791153,-20.0822650788901));
#18660=CARTESIAN_POINT('Ctrl Pts',(13.9754027621768,-35.6255845401679,-19.7657545358289));
#18661=CARTESIAN_POINT('Ctrl Pts',(14.214781365486,-35.8647126834784,-19.1045289473902));
#18662=CARTESIAN_POINT('Ctrl Pts',(14.2116652821764,-35.8616652821725,-18.4999999968019));
#18663=CARTESIAN_POINT('Ctrl Pts',(14.047067407583,-35.1102188374757,-20.0001437555207));
#18664=CARTESIAN_POINT('Ctrl Pts',(14.209895391559,-35.3704012871737,-19.6998305081926));
#18665=CARTESIAN_POINT('Ctrl Pts',(14.3737201797862,-35.6599355358214,-19.0761517589311));
#18666=CARTESIAN_POINT('Ctrl Pts',(14.336828593787,-35.7091509646218,-18.499999996955));
#18667=CARTESIAN_POINT('Ctrl Pts',(14.2951361405339,-34.8600966184017,-19.7669964902508));
#18668=CARTESIAN_POINT('Ctrl Pts',(14.3844114694822,-35.1434675131167,-19.5204897565762));
#18669=CARTESIAN_POINT('Ctrl Pts',(14.4661360608765,-35.4491208871255,-18.9989428562544));
#18670=CARTESIAN_POINT('Ctrl Pts',(14.4298332811648,-35.5351496535811,-18.4999999973626));
#18671=CARTESIAN_POINT('Ctrl Pts',(14.4611328976566,-34.6870356567945,-19.4146293224298));
#18672=CARTESIAN_POINT('Ctrl Pts',(14.4825401228378,-34.9711630725361,-19.2709716881243));
#18673=CARTESIAN_POINT('Ctrl Pts',(14.4987564117522,-35.2718703326553,-18.8811859318064));
#18674=CARTESIAN_POINT('Ctrl Pts',(14.4871343803803,-35.3462559207454,-18.4999999979862));
#18675=CARTESIAN_POINT('Ctrl Pts',(14.5000565697469,-34.6491729026552,-19.1402100483601));
#18676=CARTESIAN_POINT('Ctrl Pts',(14.5000254205555,-34.9088403997342,-19.0884200031548));
#18677=CARTESIAN_POINT('Ctrl Pts',(14.5000018196169,-35.1881172092201,-18.7897579239482));
#18678=CARTESIAN_POINT('Ctrl Pts',(14.5000187262999,-35.2152595935161,-18.4999999984667));
#18679=CARTESIAN_POINT('Ctrl Pts',(14.4999998765827,-34.6443207244513,-18.9995579554883));
#18680=CARTESIAN_POINT('Ctrl Pts',(14.499999944535,-34.8868464995459,-18.9943613932121));
#18681=CARTESIAN_POINT('Ctrl Pts',(14.4999999960227,-35.1498332908573,-18.7428715921071));
#18682=CARTESIAN_POINT('Ctrl Pts',(14.499999959143,-35.149714618927,-18.4999999987146));
#18683=CARTESIAN_POINT('Ctrl Pts',(14.5000000000013,5.14433809692412,-19.0000100692486));
#18684=CARTESIAN_POINT('Ctrl Pts',(14.5000000000008,5.38710591139172,-19.0015933091117));
#18685=CARTESIAN_POINT('Ctrl Pts',(14.5000000000027,5.65000000092752,-18.7430757267142));
#18686=CARTESIAN_POINT('Ctrl Pts',(14.5000000000019,5.65,-18.4999999987137));
#18687=CARTESIAN_POINT('Ctrl Pts',(14.5000000000024,5.14531732835656,-19.1412652085418));
#18688=CARTESIAN_POINT('Ctrl Pts',(14.5000000000012,5.40648310443134,-19.0954746833587));
#18689=CARTESIAN_POINT('Ctrl Pts',(14.5000000000026,5.6869365607798,-18.7901585471388));
#18690=CARTESIAN_POINT('Ctrl Pts',(14.5000000000012,5.71544984710073,-18.4999999984638));
#18691=CARTESIAN_POINT('Ctrl Pts',(14.4610889502624,5.18969473946802,-19.4141933256432));
#18692=CARTESIAN_POINT('Ctrl Pts',(14.4808879882489,5.47328907376343,-19.2739493035041));
#18693=CARTESIAN_POINT('Ctrl Pts',(14.4987197414756,5.77268812181769,-18.8825190881872));
#18694=CARTESIAN_POINT('Ctrl Pts',(14.4871066327078,5.84634739127338,-18.4999999979725));
#18695=CARTESIAN_POINT('Ctrl Pts',(14.2951753510102,5.3592320493172,-19.7671081794728));
#18696=CARTESIAN_POINT('Ctrl Pts',(14.3829355447185,5.64264909049228,-19.5234352013663));
#18697=CARTESIAN_POINT('Ctrl Pts',(14.4661265700051,5.94892750840517,-18.9987393235421));
#18698=CARTESIAN_POINT('Ctrl Pts',(14.4298332811675,6.03514965358259,-18.4999999973609));
#18699=CARTESIAN_POINT('Ctrl Pts',(14.0470778370448,5.61048016122898,-20.0000694996515));
#18700=CARTESIAN_POINT('Ctrl Pts',(14.2086929929188,5.8704167792382,-19.7008597170397));
#18701=CARTESIAN_POINT('Ctrl Pts',(14.373854422343,6.15979505035749,-19.0757337060927));
#18702=CARTESIAN_POINT('Ctrl Pts',(14.3368285937893,6.20915096462677,-18.4999999969561));
#18703=CARTESIAN_POINT('Ctrl Pts',(13.754269179114,5.90420357340269,-20.0822650788921));
#18704=CARTESIAN_POINT('Ctrl Pts',(13.9755845401674,6.12540276217445,-19.7657545358308));
#18705=CARTESIAN_POINT('Ctrl Pts',(14.2147126834794,6.36478136548791,-19.1045289473886));
#18706=CARTESIAN_POINT('Ctrl Pts',(14.2116652821725,6.36166528217614,-18.4999999967981));
#18707=CARTESIAN_POINT('Ctrl Pts',(13.4602188374814,6.19706740757966,-20.0001437555225));
#18708=CARTESIAN_POINT('Ctrl Pts',(13.7204012871739,6.35989539155808,-19.6998305081945));
#18709=CARTESIAN_POINT('Ctrl Pts',(14.0099355358226,6.52372017978849,-19.0761517589296));
#18710=CARTESIAN_POINT('Ctrl Pts',(14.0591509646221,6.48682859378936,-18.4999999969514));
#18711=CARTESIAN_POINT('Ctrl Pts',(13.2100966183999,6.44513614053531,-19.7669964902523));
#18712=CARTESIAN_POINT('Ctrl Pts',(13.493467513116,6.53441146948378,-19.5204897565778));
#18713=CARTESIAN_POINT('Ctrl Pts',(13.7991208871266,6.61613606087756,-18.9989428562532));
#18714=CARTESIAN_POINT('Ctrl Pts',(13.8851496535816,6.57983328116744,-18.4999999973594));
#18715=CARTESIAN_POINT('Ctrl Pts',(13.0371194604117,6.61105251483121,-19.4147999538868));
#18716=CARTESIAN_POINT('Ctrl Pts',(13.3212465098142,6.63249260469108,-19.2710925155897));
#18717=CARTESIAN_POINT('Ctrl Pts',(13.6219561650578,6.64874061556663,-18.8812429548125));
#18718=CARTESIAN_POINT('Ctrl Pts',(13.6963473912789,6.63710663270717,-18.4999999979835));
#18719=CARTESIAN_POINT('Ctrl Pts',(12.9992279345896,6.64999999999977,-19.1406085881775));
#18720=CARTESIAN_POINT('Ctrl Pts',(13.2589309435617,6.65000000000017,-19.0886851287518));
#18721=CARTESIAN_POINT('Ctrl Pts',(13.5382388686105,6.65000000000027,-18.7898907052046));
#18722=CARTESIAN_POINT('Ctrl Pts',(13.5654498470941,6.65000000000003,-18.4999999984642));
#18723=CARTESIAN_POINT('Ctrl Pts',(12.9943419397744,6.64999999999998,-19.0001703298077));
#18724=CARTESIAN_POINT('Ctrl Pts',(13.2369423184849,6.65000000000029,-18.9947709047236));
#18725=CARTESIAN_POINT('Ctrl Pts',(13.5000000009278,6.65000000000017,-18.7430757267408));
#18726=CARTESIAN_POINT('Ctrl Pts',(13.4999999999998,6.65000000000004,-18.499999998712));
#18727=CARTESIAN_POINT('Origin',(13.98,-23.05,-5.));
#18728=CARTESIAN_POINT('',(13.98,-37.95,-4.1));
#18729=CARTESIAN_POINT('',(13.98,-23.05,-4.1));
#18730=CARTESIAN_POINT('',(13.98,-23.05,-4.1));
#18731=CARTESIAN_POINT('',(13.98,-23.05,-5.));
#18732=CARTESIAN_POINT('',(13.98,-37.95,-5.));
#18733=CARTESIAN_POINT('Origin',(18.88,-23.05,-5.));
#18734=CARTESIAN_POINT('',(18.88,-23.05,-4.1));
#18735=CARTESIAN_POINT('',(18.88,-23.05,-4.1));
#18736=CARTESIAN_POINT('',(18.88,-23.05,-5.));
#18737=CARTESIAN_POINT('Origin',(18.88,-37.95,-5.));
#18738=CARTESIAN_POINT('',(18.88,-37.95,-4.1));
#18739=CARTESIAN_POINT('',(18.88,-37.95,-4.1));
#18740=CARTESIAN_POINT('',(18.88,-37.95,-5.));
#18741=CARTESIAN_POINT('Origin',(13.98,-37.95,-5.));
#18742=CARTESIAN_POINT('',(13.98,-37.95,-4.1));
#18743=CARTESIAN_POINT('Origin',(0.,0.,28.));
#18744=CARTESIAN_POINT('Origin',(0.,0.,-4.1));
#18745=CARTESIAN_POINT('Origin',(0.,0.,-19.8));
#18746=CARTESIAN_POINT('Origin',(0.,0.,-4.1));
#18747=CARTESIAN_POINT('Origin',(0.,0.,-21.));
#18748=CARTESIAN_POINT('Origin',(0.,0.,-23.5));
#18749=CARTESIAN_POINT('Origin',(0.,0.,-24.3));
#18750=CARTESIAN_POINT('Origin',(0.,0.,-26.1));
#18751=CARTESIAN_POINT('',(0.,0.,0.));
#18752=CARTESIAN_POINT('Origin',(-6.,0.,-11.));
#18753=CARTESIAN_POINT('',(-6.,0.,-12.25));
#18754=CARTESIAN_POINT('Origin',(-6.,0.,-11.));
#18755=CARTESIAN_POINT('',(-6.,2.,-12.25));
#18756=CARTESIAN_POINT('',(-6.,0.,-12.25));
#18757=CARTESIAN_POINT('Origin',(-6.,2.,-11.));
#18758=CARTESIAN_POINT('Origin',(-11.,0.,6.));
#18759=CARTESIAN_POINT('',(-11.,0.,4.75));
#18760=CARTESIAN_POINT('Origin',(-11.,0.,6.));
#18761=CARTESIAN_POINT('',(-11.,2.,4.75));
#18762=CARTESIAN_POINT('',(-11.,0.,4.75));
#18763=CARTESIAN_POINT('Origin',(-11.,2.,6.));
#18764=CARTESIAN_POINT('Origin',(6.,0.,11.));
#18765=CARTESIAN_POINT('',(6.,0.,9.75));
#18766=CARTESIAN_POINT('Origin',(6.,0.,11.));
#18767=CARTESIAN_POINT('',(6.,2.,9.75));
#18768=CARTESIAN_POINT('',(6.,0.,9.75));
#18769=CARTESIAN_POINT('Origin',(6.,2.,11.));
#18770=CARTESIAN_POINT('Origin',(11.,0.,-6.));
#18771=CARTESIAN_POINT('',(11.,0.,-7.25));
#18772=CARTESIAN_POINT('Origin',(11.,0.,-6.));
#18773=CARTESIAN_POINT('',(11.,2.,-7.25));
#18774=CARTESIAN_POINT('',(11.,0.,-7.25));
#18775=CARTESIAN_POINT('Origin',(11.,2.,-6.));
#18776=CARTESIAN_POINT('Origin',(-11.,10.74803620541,-6.));
#18777=CARTESIAN_POINT('',(-11.,2.,-4.975));
#18778=CARTESIAN_POINT('Origin',(-11.,2.,-6.));
#18779=CARTESIAN_POINT('',(-11.,0.325,-4.975));
#18780=CARTESIAN_POINT('',(-11.,10.74803620541,-4.975));
#18781=CARTESIAN_POINT('Origin',(-11.,0.325000000000001,-6.));
#18782=CARTESIAN_POINT('Origin',(-6.,10.74803620541,11.));
#18783=CARTESIAN_POINT('',(-6.,2.,12.025));
#18784=CARTESIAN_POINT('Origin',(-6.,2.,11.));
#18785=CARTESIAN_POINT('',(-6.,0.325,12.025));
#18786=CARTESIAN_POINT('',(-6.,10.74803620541,12.025));
#18787=CARTESIAN_POINT('Origin',(-6.,0.325000000000001,11.));
#18788=CARTESIAN_POINT('Origin',(11.,10.74803620541,6.));
#18789=CARTESIAN_POINT('',(11.,2.,7.025));
#18790=CARTESIAN_POINT('Origin',(11.,2.,6.));
#18791=CARTESIAN_POINT('',(11.,0.325,7.025));
#18792=CARTESIAN_POINT('',(11.,10.74803620541,7.025));
#18793=CARTESIAN_POINT('Origin',(11.,0.325000000000001,6.));
#18794=CARTESIAN_POINT('Origin',(6.,10.74803620541,-11.));
#18795=CARTESIAN_POINT('',(6.,2.,-9.975));
#18796=CARTESIAN_POINT('Origin',(6.,2.,-11.));
#18797=CARTESIAN_POINT('',(6.,0.325,-9.975));
#18798=CARTESIAN_POINT('',(6.,10.74803620541,-9.975));
#18799=CARTESIAN_POINT('Origin',(6.,0.325000000000001,-11.));
#18800=CARTESIAN_POINT('Origin',(3.5,0.,-8.));
#18801=CARTESIAN_POINT('',(3.5,0.,-9.25));
#18802=CARTESIAN_POINT('Origin',(3.5,0.,-8.));
#18803=CARTESIAN_POINT('',(3.5,2.,-9.25));
#18804=CARTESIAN_POINT('',(3.5,0.,-9.25));
#18805=CARTESIAN_POINT('Origin',(3.5,2.,-8.));
#18806=CARTESIAN_POINT('Origin',(-8.,0.,-3.5));
#18807=CARTESIAN_POINT('',(-8.,0.,-4.75));
#18808=CARTESIAN_POINT('Origin',(-8.,0.,-3.5));
#18809=CARTESIAN_POINT('',(-8.,2.,-4.75));
#18810=CARTESIAN_POINT('',(-8.,0.,-4.75));
#18811=CARTESIAN_POINT('Origin',(-8.,2.,-3.5));
#18812=CARTESIAN_POINT('Origin',(-3.5,0.,8.));
#18813=CARTESIAN_POINT('',(-3.5,0.,6.75));
#18814=CARTESIAN_POINT('Origin',(-3.5,0.,8.));
#18815=CARTESIAN_POINT('',(-3.5,2.,6.75));
#18816=CARTESIAN_POINT('',(-3.5,0.,6.75));
#18817=CARTESIAN_POINT('Origin',(-3.5,2.,8.));
#18818=CARTESIAN_POINT('Origin',(8.,0.,3.5));
#18819=CARTESIAN_POINT('',(8.,0.,2.25));
#18820=CARTESIAN_POINT('Origin',(8.,0.,3.5));
#18821=CARTESIAN_POINT('',(8.,2.,2.25));
#18822=CARTESIAN_POINT('',(8.,0.,2.25));
#18823=CARTESIAN_POINT('Origin',(8.,2.,3.5));
#18824=CARTESIAN_POINT('Origin',(-3.5,10.74803620541,-8.));
#18825=CARTESIAN_POINT('',(-3.5,2.,-6.975));
#18826=CARTESIAN_POINT('Origin',(-3.5,2.,-8.));
#18827=CARTESIAN_POINT('',(-3.5,0.325,-6.975));
#18828=CARTESIAN_POINT('',(-3.5,10.74803620541,-6.975));
#18829=CARTESIAN_POINT('Origin',(-3.5,0.325000000000001,-8.));
#18830=CARTESIAN_POINT('Origin',(-8.,10.74803620541,3.5));
#18831=CARTESIAN_POINT('',(-8.,2.,4.525));
#18832=CARTESIAN_POINT('Origin',(-8.,2.,3.5));
#18833=CARTESIAN_POINT('',(-8.,0.325,4.525));
#18834=CARTESIAN_POINT('',(-8.,10.74803620541,4.525));
#18835=CARTESIAN_POINT('Origin',(-8.,0.325000000000001,3.5));
#18836=CARTESIAN_POINT('Origin',(3.5,10.74803620541,8.));
#18837=CARTESIAN_POINT('',(3.5,2.,9.025));
#18838=CARTESIAN_POINT('Origin',(3.5,2.,8.));
#18839=CARTESIAN_POINT('',(3.5,0.325,9.025));
#18840=CARTESIAN_POINT('',(3.5,10.74803620541,9.025));
#18841=CARTESIAN_POINT('Origin',(3.5,0.325000000000001,8.));
#18842=CARTESIAN_POINT('Origin',(8.,10.74803620541,-3.5));
#18843=CARTESIAN_POINT('',(8.,2.,-2.475));
#18844=CARTESIAN_POINT('Origin',(8.,2.,-3.5));
#18845=CARTESIAN_POINT('',(8.,0.325,-2.475));
#18846=CARTESIAN_POINT('',(8.,10.74803620541,-2.475));
#18847=CARTESIAN_POINT('Origin',(8.,0.325000000000001,-3.5));
#18848=CARTESIAN_POINT('Origin',(7.778174593052,2.,-7.778174593052));
#18849=CARTESIAN_POINT('',(7.778174593052,2.,-6.528174593052));
#18850=CARTESIAN_POINT('Origin',(7.778174593052,2.,-7.778174593052));
#18851=CARTESIAN_POINT('',(7.778174593052,0.,-6.528174593052));
#18852=CARTESIAN_POINT('',(7.778174593052,2.,-6.528174593052));
#18853=CARTESIAN_POINT('Origin',(7.778174593052,0.,-7.778174593052));
#18854=CARTESIAN_POINT('Origin',(0.,2.,-11.));
#18855=CARTESIAN_POINT('',(-1.53080849893419E-16,2.,-9.75));
#18856=CARTESIAN_POINT('Origin',(0.,2.,-11.));
#18857=CARTESIAN_POINT('',(-1.53080849893419E-16,0.,-9.75));
#18858=CARTESIAN_POINT('',(-1.53080849893419E-16,2.,-9.75));
#18859=CARTESIAN_POINT('Origin',(0.,0.,-11.));
#18860=CARTESIAN_POINT('Origin',(-7.778174593052,2.,-7.778174593052));
#18861=CARTESIAN_POINT('',(-7.778174593052,2.,-6.528174593052));
#18862=CARTESIAN_POINT('Origin',(-7.778174593052,2.,-7.778174593052));
#18863=CARTESIAN_POINT('',(-7.778174593052,0.,-6.528174593052));
#18864=CARTESIAN_POINT('',(-7.778174593052,2.,-6.528174593052));
#18865=CARTESIAN_POINT('Origin',(-7.778174593052,0.,-7.778174593052));
#18866=CARTESIAN_POINT('Origin',(-11.,2.,0.));
#18867=CARTESIAN_POINT('',(-11.,2.,1.25));
#18868=CARTESIAN_POINT('Origin',(-11.,2.,0.));
#18869=CARTESIAN_POINT('',(-11.,0.,1.25));
#18870=CARTESIAN_POINT('',(-11.,2.,1.25));
#18871=CARTESIAN_POINT('Origin',(-11.,0.,0.));
#18872=CARTESIAN_POINT('Origin',(-7.778174593052,2.,7.778174593052));
#18873=CARTESIAN_POINT('',(-7.778174593052,2.,9.028174593052));
#18874=CARTESIAN_POINT('Origin',(-7.778174593052,2.,7.778174593052));
#18875=CARTESIAN_POINT('',(-7.778174593052,0.,9.028174593052));
#18876=CARTESIAN_POINT('',(-7.778174593052,2.,9.028174593052));
#18877=CARTESIAN_POINT('Origin',(-7.778174593052,0.,7.778174593052));
#18878=CARTESIAN_POINT('Origin',(0.,2.,11.));
#18879=CARTESIAN_POINT('',(-1.53080849893419E-16,2.,12.25));
#18880=CARTESIAN_POINT('Origin',(0.,2.,11.));
#18881=CARTESIAN_POINT('',(-1.53080849893419E-16,0.,12.25));
#18882=CARTESIAN_POINT('',(-1.53080849893419E-16,2.,12.25));
#18883=CARTESIAN_POINT('Origin',(0.,0.,11.));
#18884=CARTESIAN_POINT('Origin',(7.778174593052,2.,7.778174593052));
#18885=CARTESIAN_POINT('',(7.778174593052,2.,9.028174593052));
#18886=CARTESIAN_POINT('Origin',(7.778174593052,2.,7.778174593052));
#18887=CARTESIAN_POINT('',(7.778174593052,0.,9.028174593052));
#18888=CARTESIAN_POINT('',(7.778174593052,2.,9.028174593052));
#18889=CARTESIAN_POINT('Origin',(7.778174593052,0.,7.778174593052));
#18890=CARTESIAN_POINT('Origin',(11.,2.,0.));
#18891=CARTESIAN_POINT('',(11.,2.,1.25));
#18892=CARTESIAN_POINT('Origin',(11.,2.,0.));
#18893=CARTESIAN_POINT('',(11.,0.,1.25));
#18894=CARTESIAN_POINT('',(11.,2.,1.25));
#18895=CARTESIAN_POINT('Origin',(11.,0.,0.));
#18896=CARTESIAN_POINT('Origin',(0.,1.,0.));
#18897=CARTESIAN_POINT('',(-6.12323399573677E-16,2.,5.));
#18898=CARTESIAN_POINT('Origin',(0.,2.,0.));
#18899=CARTESIAN_POINT('',(-6.12323399573677E-16,0.1999518233597,5.));
#18900=CARTESIAN_POINT('',(-6.12323399573677E-16,1.,5.));
#18901=CARTESIAN_POINT('Origin',(0.,0.1999518233597,4.25007251614318E-14));
#18902=CARTESIAN_POINT('Origin',(-11.,5.6843418860808E-11,-6.));
#18903=CARTESIAN_POINT('',(-11.,-5.68436964165642E-11,-4.64999999996962));
#18904=CARTESIAN_POINT('',(-11.,5.6843418860808E-11,-4.65000000008331));
#18905=CARTESIAN_POINT('Origin',(-11.,-5.6843418860808E-11,-6.));
#18906=CARTESIAN_POINT('Origin',(-6.,5.6843418860808E-11,11.));
#18907=CARTESIAN_POINT('',(-6.,-5.68436964165642E-11,12.3500000000304));
#18908=CARTESIAN_POINT('',(-6.,5.6843418860808E-11,12.3499999999167));
#18909=CARTESIAN_POINT('Origin',(-6.,-5.6843418860808E-11,11.));
#18910=CARTESIAN_POINT('Origin',(11.,5.6843418860808E-11,6.));
#18911=CARTESIAN_POINT('',(11.,-5.6843505617991E-11,7.35000000003038));
#18912=CARTESIAN_POINT('',(11.,5.6843418860808E-11,7.34999999991669));
#18913=CARTESIAN_POINT('Origin',(11.,-5.6843418860808E-11,6.));
#18914=CARTESIAN_POINT('Origin',(6.,5.6843418860808E-11,-11.));
#18915=CARTESIAN_POINT('',(6.,-5.68436964165642E-11,-9.64999999996962));
#18916=CARTESIAN_POINT('',(6.,5.6843418860808E-11,-9.65000000008331));
#18917=CARTESIAN_POINT('Origin',(6.,-5.6843418860808E-11,-11.));
#18918=CARTESIAN_POINT('Origin',(-3.5,5.6843418860808E-11,-8.));
#18919=CARTESIAN_POINT('',(-3.5,-5.68435576386861E-11,-6.64999999997917));
#18920=CARTESIAN_POINT('',(-3.5,5.6843418860808E-11,-6.65000000009286));
#18921=CARTESIAN_POINT('Origin',(-3.5,-5.6843418860808E-11,-8.));
#18922=CARTESIAN_POINT('Origin',(-8.,5.6843418860808E-11,3.5));
#18923=CARTESIAN_POINT('',(-8.,-5.68435569810944E-11,4.85000000002083));
#18924=CARTESIAN_POINT('',(-8.,5.6843418860808E-11,4.84999999990714));
#18925=CARTESIAN_POINT('Origin',(-8.,-5.6843418860808E-11,3.5));
#18926=CARTESIAN_POINT('Origin',(3.5,5.6843418860808E-11,8.));
#18927=CARTESIAN_POINT('',(3.5,-5.68435576386861E-11,9.35000000002083));
#18928=CARTESIAN_POINT('',(3.5,5.6843418860808E-11,9.34999999990714));
#18929=CARTESIAN_POINT('Origin',(3.5,-5.6843418860808E-11,8.));
#18930=CARTESIAN_POINT('Origin',(8.,5.6843418860808E-11,-3.5));
#18931=CARTESIAN_POINT('',(8.,-5.68435227390255E-11,-2.14999999997917));
#18932=CARTESIAN_POINT('',(8.,5.6843418860808E-11,-2.15000000009286));
#18933=CARTESIAN_POINT('Origin',(8.,-5.6843418860808E-11,-3.5));
#18934=CARTESIAN_POINT('Origin',(0.,-2.12617692341155E-5,4.25007251614318E-14));
#18935=CARTESIAN_POINT('',(-6.36810199687457E-16,-4.58884334339753E-15,
5.19994989682604));
#18936=CARTESIAN_POINT('',(-6.36812803478132E-16,-2.12617692341155E-5,5.19997115839041));
#18937=CARTESIAN_POINT('Origin',(-1.7763568394E-14,0.,0.));
#18938=CARTESIAN_POINT('Origin',(-11.,6.7,19.));
#18939=CARTESIAN_POINT('',(-9.7,6.7,19.));
#18940=CARTESIAN_POINT('Origin',(-11.,6.7,19.));
#18941=CARTESIAN_POINT('',(-9.7,6.7,17.));
#18942=CARTESIAN_POINT('',(-9.7,6.7,19.));
#18943=CARTESIAN_POINT('Origin',(-11.,6.7,17.));
#18944=CARTESIAN_POINT('Origin',(11.,6.7,19.));
#18945=CARTESIAN_POINT('',(12.3,6.7,19.));
#18946=CARTESIAN_POINT('Origin',(11.,6.7,19.));
#18947=CARTESIAN_POINT('',(12.3,6.7,17.));
#18948=CARTESIAN_POINT('',(12.3,6.7,19.));
#18949=CARTESIAN_POINT('Origin',(11.,6.7,17.));
#18950=CARTESIAN_POINT('Origin',(-18.,6.7,19.));
#18951=CARTESIAN_POINT('',(-16.7,6.7,19.));
#18952=CARTESIAN_POINT('Origin',(-18.,6.7,19.));
#18953=CARTESIAN_POINT('',(-16.7,6.7,17.));
#18954=CARTESIAN_POINT('',(-16.7,6.7,19.));
#18955=CARTESIAN_POINT('Origin',(-18.,6.7,17.));
#18956=CARTESIAN_POINT('Origin',(4.,6.7,19.));
#18957=CARTESIAN_POINT('',(5.3,6.7,19.));
#18958=CARTESIAN_POINT('Origin',(4.,6.7,19.));
#18959=CARTESIAN_POINT('',(5.3,6.7,17.));
#18960=CARTESIAN_POINT('',(5.3,6.7,19.));
#18961=CARTESIAN_POINT('Origin',(4.,6.7,17.));
#18962=CARTESIAN_POINT('Origin',(-11.,6.7,19.));
#18963=CARTESIAN_POINT('',(-9.7,6.7,-17.));
#18964=CARTESIAN_POINT('Origin',(-11.,6.7,-17.));
#18965=CARTESIAN_POINT('',(-9.7,6.7,-19.));
#18966=CARTESIAN_POINT('',(-9.7,6.7,19.));
#18967=CARTESIAN_POINT('Origin',(-11.,6.7,-19.));
#18968=CARTESIAN_POINT('Origin',(11.,6.7,19.));
#18969=CARTESIAN_POINT('',(12.3,6.7,-17.));
#18970=CARTESIAN_POINT('Origin',(11.,6.7,-17.));
#18971=CARTESIAN_POINT('',(12.3,6.7,-19.));
#18972=CARTESIAN_POINT('',(12.3,6.7,19.));
#18973=CARTESIAN_POINT('Origin',(11.,6.7,-19.));
#18974=CARTESIAN_POINT('Origin',(-18.,6.7,19.));
#18975=CARTESIAN_POINT('',(-16.7,6.7,-17.));
#18976=CARTESIAN_POINT('Origin',(-18.,6.7,-17.));
#18977=CARTESIAN_POINT('',(-16.7,6.7,-19.));
#18978=CARTESIAN_POINT('',(-16.7,6.7,19.));
#18979=CARTESIAN_POINT('Origin',(-18.,6.7,-19.));
#18980=CARTESIAN_POINT('Origin',(4.,6.7,19.));
#18981=CARTESIAN_POINT('',(5.3,6.7,-17.));
#18982=CARTESIAN_POINT('Origin',(4.,6.7,-17.));
#18983=CARTESIAN_POINT('',(5.3,6.7,-19.));
#18984=CARTESIAN_POINT('',(5.3,6.7,19.));
#18985=CARTESIAN_POINT('Origin',(4.,6.7,-19.));
#18986=CARTESIAN_POINT('Origin',(14.5,2.,16.5));
#18987=CARTESIAN_POINT('',(14.5,2.,-16.5));
#18988=CARTESIAN_POINT('',(14.5,2.,16.5));
#18989=CARTESIAN_POINT('',(14.5,2.,16.5));
#18990=CARTESIAN_POINT('',(-15.6010205144338,2.,-16.4999999999986));
#18991=CARTESIAN_POINT('',(14.5,2.,-16.5));
#18992=CARTESIAN_POINT('',(-14.5,2.,-13.03589838486));
#18993=CARTESIAN_POINT('Origin',(-20.5,2.,-13.03589838486));
#18994=CARTESIAN_POINT('',(-14.5,2.,13.03589838486));
#18995=CARTESIAN_POINT('',(-14.5,2.,16.5));
#18996=CARTESIAN_POINT('',(-15.6010205144317,2.,16.5000000000002));
#18997=CARTESIAN_POINT('Origin',(-20.5,2.,13.03589838486));
#18998=CARTESIAN_POINT('',(14.5,2.,16.5));
#18999=CARTESIAN_POINT('Origin',(14.5,2.5,16.5));
#19000=CARTESIAN_POINT('',(14.5,2.5,17.));
#19001=CARTESIAN_POINT('Origin',(14.5,2.5,16.5));
#19002=CARTESIAN_POINT('',(-17.5000000000001,2.47654106818559,16.9994493753306));
#19003=CARTESIAN_POINT('Ctrl Pts',(-17.5000096922892,2.47654352708651,16.9994494908181));
#19004=CARTESIAN_POINT('Ctrl Pts',(-17.371522845629,2.44394677638692,16.9979184348396));
#19005=CARTESIAN_POINT('Ctrl Pts',(-17.2437747299337,2.40878815792915,16.993079083846));
#19006=CARTESIAN_POINT('Ctrl Pts',(-16.9941658745484,2.33637313275275,16.9739051828542));
#19007=CARTESIAN_POINT('Ctrl Pts',(-16.8736840331451,2.29951631658164,16.9600004544787));
#19008=CARTESIAN_POINT('Ctrl Pts',(-16.6759259011892,2.2383018761184,16.9269138033769));
#19009=CARTESIAN_POINT('Ctrl Pts',(-16.5989139658977,2.21432329962625,16.9114276432015));
#19010=CARTESIAN_POINT('Ctrl Pts',(-16.4372876162009,2.1648760551481,16.8725483781765));
#19011=CARTESIAN_POINT('Ctrl Pts',(-16.3536394704351,2.13973650391793,16.8486261868388));
#19012=CARTESIAN_POINT('Ctrl Pts',(-16.1512480291796,2.08295164252046,16.7806829189119));
#19013=CARTESIAN_POINT('Ctrl Pts',(-16.0338807886608,2.05340445436661,16.7327203097712));
#19014=CARTESIAN_POINT('Ctrl Pts',(-15.8101466828132,2.01228090697128,16.6237475601439));
#19015=CARTESIAN_POINT('Ctrl Pts',(-15.7042606821881,2.00000000000037,16.5642271272144));
#19016=CARTESIAN_POINT('Ctrl Pts',(-15.60102051443,2.,16.5000000000029));
#19017=CARTESIAN_POINT('',(-17.5924003307403,2.49999999999975,17.));
#19018=CARTESIAN_POINT('Origin',(-17.5462001500739,2.63349307091694,10.8126318152261));
#19019=CARTESIAN_POINT('',(14.5,2.5,17.));
#19020=CARTESIAN_POINT('Origin',(14.5,1.,0.));
#19021=CARTESIAN_POINT('',(14.5,7.3,17.));
#19022=CARTESIAN_POINT('',(14.5,9.3,17.));
#19023=CARTESIAN_POINT('',(14.5,7.3,19.));
#19024=CARTESIAN_POINT('',(14.5,7.3,18.));
#19025=CARTESIAN_POINT('',(14.5,2.5,19.));
#19026=CARTESIAN_POINT('',(14.5,5.9,19.));
#19027=CARTESIAN_POINT('',(14.5,0.,16.5));
#19028=CARTESIAN_POINT('Origin',(14.5,2.5,16.5));
#19029=CARTESIAN_POINT('',(14.5,0.,-16.5));
#19030=CARTESIAN_POINT('',(14.5,0.,0.));
#19031=CARTESIAN_POINT('',(14.5,2.5,-19.));
#19032=CARTESIAN_POINT('Origin',(14.5,2.5,-16.5));
#19033=CARTESIAN_POINT('',(14.5,7.3,-19.));
#19034=CARTESIAN_POINT('',(14.5,5.9,-19.));
#19035=CARTESIAN_POINT('',(14.5,7.3,-17.));
#19036=CARTESIAN_POINT('',(14.5,7.3,-18.));
#19037=CARTESIAN_POINT('',(14.5,2.5,-17.));
#19038=CARTESIAN_POINT('',(14.5,2.5,-17.));
#19039=CARTESIAN_POINT('Origin',(14.5,2.5,-16.5));
#19040=CARTESIAN_POINT('Origin',(14.5,2.5,-16.5));
#19041=CARTESIAN_POINT('',(-17.59240033074,2.49999999999972,-17.));
#19042=CARTESIAN_POINT('',(14.5,2.5,-17.));
#19043=CARTESIAN_POINT('',(-17.4999999999994,2.47654106818636,-16.9994493753306));
#19044=CARTESIAN_POINT('Origin',(-17.5462001542397,2.63349226331312,-10.8126669805471));
#19045=CARTESIAN_POINT('Ctrl Pts',(-15.6010120234613,2.0000000000279,-16.4999947176331));
#19046=CARTESIAN_POINT('Ctrl Pts',(-15.704076554021,2.00000000002768,-16.5641125785337));
#19047=CARTESIAN_POINT('Ctrl Pts',(-15.8097881082795,2.01223958419737,-16.6235460520593));
#19048=CARTESIAN_POINT('Ctrl Pts',(-16.0331149291658,2.05323764858778,-16.7323757326034));
#19049=CARTESIAN_POINT('Ctrl Pts',(-16.1502586572613,2.08269792549789,-16.78029277891));
#19050=CARTESIAN_POINT('Ctrl Pts',(-16.3522616768077,2.13933342892633,-16.8482037730104));
#19051=CARTESIAN_POINT('Ctrl Pts',(-16.435747260524,2.16441192529145,-16.8721268381227));
#19052=CARTESIAN_POINT('Ctrl Pts',(-16.5973270171487,2.21383152604932,-16.9110908172613));
#19053=CARTESIAN_POINT('Ctrl Pts',(-16.6744641820304,2.23784785033491,-16.926638975002));
#19054=CARTESIAN_POINT('Ctrl Pts',(-16.8725510272894,2.29916800021421,-16.9598573262036));
#19055=CARTESIAN_POINT('Ctrl Pts',(-16.9932348770165,2.33609618849181,-16.9738155944474));
#19056=CARTESIAN_POINT('Ctrl Pts',(-17.2432994237094,2.4086572889119,-16.9930611081183));
#19057=CARTESIAN_POINT('Ctrl Pts',(-17.3712742011148,2.44388369598067,-16.997915471985));
#19058=CARTESIAN_POINT('Ctrl Pts',(-17.4999999999993,2.47654106818655,-16.9994493753306));
#19059=CARTESIAN_POINT('Origin',(-20.5,1.,-13.03589838486));
#19060=CARTESIAN_POINT('',(-15.6010205144335,1.36338022765876,-16.4999999999975));
#19061=CARTESIAN_POINT('',(-15.6010205144335,1.,-16.4999999999975));
#19062=CARTESIAN_POINT('',(-15.6010205144328,-2.57498015965307E-16,-16.4999999999996));
#19063=CARTESIAN_POINT('',(-15.6010205144335,1.,-16.4999999999975));
#19064=CARTESIAN_POINT('',(-14.5,0.,-13.03589838486));
#19065=CARTESIAN_POINT('Origin',(-20.5,0.,-13.03589838486));
#19066=CARTESIAN_POINT('',(-14.5,1.,-13.03589838486));
#19067=CARTESIAN_POINT('Origin',(-14.5,1.,0.));
#19068=CARTESIAN_POINT('',(-14.5,0.,13.03589838486));
#19069=CARTESIAN_POINT('',(-14.5,0.,0.));
#19070=CARTESIAN_POINT('',(-14.5,1.,13.03589838486));
#19071=CARTESIAN_POINT('Origin',(-20.5,1.,13.03589838486));
#19072=CARTESIAN_POINT('',(-15.6010205144326,0.,16.5));
#19073=CARTESIAN_POINT('Origin',(-20.5,0.,13.03589838486));
#19074=CARTESIAN_POINT('',(-15.6010205144335,1.36338022760973,16.4999999999975));
#19075=CARTESIAN_POINT('',(-15.6010205144335,1.,16.4999999999975));
#19076=CARTESIAN_POINT('',(-15.6010205144335,1.,16.4999999999975));
#19077=CARTESIAN_POINT('Origin',(14.5,0.,16.5));
#19078=CARTESIAN_POINT('',(14.5,0.,16.5));
#19079=CARTESIAN_POINT('',(14.5,0.,-16.5));
#19080=CARTESIAN_POINT('Origin',(14.5,9.3,17.));
#19081=CARTESIAN_POINT('',(-20.499999999999,4.17870345174027,17.));
#19082=CARTESIAN_POINT('',(-20.5,4.17870345174,17.));
#19083=CARTESIAN_POINT('',(-21.5,5.910754259309,17.));
#19084=CARTESIAN_POINT('Origin',(-19.5,5.910754259309,17.));
#19085=CARTESIAN_POINT('',(-21.5,7.3,17.));
#19086=CARTESIAN_POINT('',(-21.5,5.9,17.));
#19087=CARTESIAN_POINT('',(-19.5,9.3,17.));
#19088=CARTESIAN_POINT('Origin',(-19.5,7.3,17.));
#19089=CARTESIAN_POINT('',(12.5,9.3,17.));
#19090=CARTESIAN_POINT('',(14.5,9.3,17.));
#19091=CARTESIAN_POINT('Origin',(12.5,7.3,17.));
#19092=CARTESIAN_POINT('Ctrl Pts',(-15.57368086877,2.074394725501,16.48538787889));
#19093=CARTESIAN_POINT('Ctrl Pts',(-15.57368086877,1.358575011107,16.46081195141));
#19094=CARTESIAN_POINT('Ctrl Pts',(-15.57368086877,0.6427552967139,16.43623602393));
#19095=CARTESIAN_POINT('Ctrl Pts',(-15.57368086877,-0.07306441767953,16.41166009645));
#19096=CARTESIAN_POINT('Ctrl Pts',(-15.58274239264,2.074223770141,16.49027240659));
#19097=CARTESIAN_POINT('Ctrl Pts',(-15.58274239264,1.358116528257,16.47391169971));
#19098=CARTESIAN_POINT('Ctrl Pts',(-15.58274239264,0.6420092863734,16.45755099284));
#19099=CARTESIAN_POINT('Ctrl Pts',(-15.58274239264,-0.07409795551055,16.44119028597));
#19100=CARTESIAN_POINT('Ctrl Pts',(-15.71578181391,2.072990731385,16.56138770748));
#19101=CARTESIAN_POINT('Ctrl Pts',(-15.71578181391,1.35480965841,16.66463485657));
#19102=CARTESIAN_POINT('Ctrl Pts',(-15.71578181391,0.6366285854352,16.76788200567));
#19103=CARTESIAN_POINT('Ctrl Pts',(-15.71578181391,-0.08155248753949,16.87112915476));
#19104=CARTESIAN_POINT('Ctrl Pts',(-15.99393964446,2.105376743577,16.6924369233));
#19105=CARTESIAN_POINT('Ctrl Pts',(-15.99393964446,1.441665263409,17.01609396359));
#19106=CARTESIAN_POINT('Ctrl Pts',(-15.99393964446,0.7779537832405,17.33975100388));
#19107=CARTESIAN_POINT('Ctrl Pts',(-15.99393964446,0.114242303072,17.66340804417));
#19108=CARTESIAN_POINT('Ctrl Pts',(-16.44881838131,2.215365528923,16.83088989051));
#19109=CARTESIAN_POINT('Ctrl Pts',(-16.44881838131,1.736642688769,17.38740909059));
#19110=CARTESIAN_POINT('Ctrl Pts',(-16.44881838131,1.257919848614,17.94392829068));
#19111=CARTESIAN_POINT('Ctrl Pts',(-16.44881838131,0.7791970084599,18.50044749077));
#19112=CARTESIAN_POINT('Ctrl Pts',(-16.95084263786,2.351489777509,16.90776164253));
#19113=CARTESIAN_POINT('Ctrl Pts',(-16.95084263786,2.101712457026,17.59357039535));
#19114=CARTESIAN_POINT('Ctrl Pts',(-16.95084263786,1.851935136544,18.27937914817));
#19115=CARTESIAN_POINT('Ctrl Pts',(-16.95084263786,1.602157816061,18.96518790099));
#19116=CARTESIAN_POINT('Ctrl Pts',(-17.32661507613,2.442923903714,16.92408316831));
#19117=CARTESIAN_POINT('Ctrl Pts',(-17.32661507613,2.346928394752,17.63734287302));
#19118=CARTESIAN_POINT('Ctrl Pts',(-17.32661507613,2.250932885791,18.35060257774));
#19119=CARTESIAN_POINT('Ctrl Pts',(-17.32661507613,2.154937376829,19.06386228246));
#19120=CARTESIAN_POINT('Ctrl Pts',(-17.52801411637,2.486045160307,16.9256422694));
#19121=CARTESIAN_POINT('Ctrl Pts',(-17.52801411637,2.462574705493,17.64152420501));
#19122=CARTESIAN_POINT('Ctrl Pts',(-17.52801411637,2.439104250679,18.35740614061));
#19123=CARTESIAN_POINT('Ctrl Pts',(-17.52801411637,2.415633795865,19.07328807622));
#19124=CARTESIAN_POINT('Ctrl Pts',(-17.54206971761,2.489025840479,16.92571861498));
#19125=CARTESIAN_POINT('Ctrl Pts',(-17.54206971761,2.470568551048,17.64172895517));
#19126=CARTESIAN_POINT('Ctrl Pts',(-17.54206971761,2.452111261618,18.35773929537));
#19127=CARTESIAN_POINT('Ctrl Pts',(-17.54206971761,2.433653972188,19.07374963557));
#19128=CARTESIAN_POINT('',(-17.5000000000011,2.38270534092832,18.997246876653));
#19129=CARTESIAN_POINT('Ctrl Pts',(-17.5000000000025,2.3827053409272,18.997246876653));
#19130=CARTESIAN_POINT('Ctrl Pts',(-17.397451060852,2.25262345741567,18.9911369840666));
#19131=CARTESIAN_POINT('Ctrl Pts',(-17.2994815869931,2.11974254320617,18.9746723858667));
#19132=CARTESIAN_POINT('Ctrl Pts',(-17.1063203414114,1.84656919417232,18.9173138353435));
#19133=CARTESIAN_POINT('Ctrl Pts',(-17.0118909483542,1.70674986776022,18.8754495661767));
#19134=CARTESIAN_POINT('Ctrl Pts',(-16.7261430930788,1.27301150209775,18.7014226944282));
#19135=CARTESIAN_POINT('Ctrl Pts',(-16.5505973550705,0.992649551630207,
18.5227840186769));
#19136=CARTESIAN_POINT('Ctrl Pts',(-16.2367523912556,0.527853643828902,
18.0679946901261));
#19137=CARTESIAN_POINT('Ctrl Pts',(-16.0994701412667,0.34318463629694,17.8048543793107));
#19138=CARTESIAN_POINT('Ctrl Pts',(-15.9050156967339,0.144535698373065,
17.35458171012));
#19139=CARTESIAN_POINT('Ctrl Pts',(-15.8415060003331,0.0917554854890558,
17.192532833357));
#19140=CARTESIAN_POINT('Ctrl Pts',(-15.7177863268808,0.0189111127370208,
16.8536222157515));
#19141=CARTESIAN_POINT('Ctrl Pts',(-15.6580928898842,3.85744012468713E-14,
16.6775275456278));
#19142=CARTESIAN_POINT('Ctrl Pts',(-15.6010205144309,-5.42101086242752E-16,
16.5000000000006));
#19143=CARTESIAN_POINT('',(-17.5000000000002,2.42961219547292,17.9985825134344));
#19144=CARTESIAN_POINT('Ctrl Pts',(-17.54192267438,2.48899465693,-16.9257178151));
#19145=CARTESIAN_POINT('Ctrl Pts',(-17.54192267438,2.470484920314,-17.64172681));
#19146=CARTESIAN_POINT('Ctrl Pts',(-17.54192267438,2.451975183698,-18.3577358049));
#19147=CARTESIAN_POINT('Ctrl Pts',(-17.54192267438,2.433465447082,-19.0737447998));
#19148=CARTESIAN_POINT('Ctrl Pts',(-17.52791631184,2.486024219187,-16.92564151185));
#19149=CARTESIAN_POINT('Ctrl Pts',(-17.52791631184,2.462518543788,-17.64152217335));
#19150=CARTESIAN_POINT('Ctrl Pts',(-17.52791631184,2.43901286839,-18.35740283484));
#19151=CARTESIAN_POINT('Ctrl Pts',(-17.52791631184,2.415507192992,-19.07328349634));
#19152=CARTESIAN_POINT('Ctrl Pts',(-17.32656780917,2.44291240257,-16.92408111528));
#19153=CARTESIAN_POINT('Ctrl Pts',(-17.32656780917,2.346897549991,-17.63733736705));
#19154=CARTESIAN_POINT('Ctrl Pts',(-17.32656780917,2.250882697412,-18.35059361882));
#19155=CARTESIAN_POINT('Ctrl Pts',(-17.32656780917,2.154867844833,-19.06384987059));
#19156=CARTESIAN_POINT('Ctrl Pts',(-16.95084263786,2.351489777509,-16.90776164253));
#19157=CARTESIAN_POINT('Ctrl Pts',(-16.95084263786,2.101712457026,-17.59357039535));
#19158=CARTESIAN_POINT('Ctrl Pts',(-16.95084263786,1.851935136544,-18.27937914817));
#19159=CARTESIAN_POINT('Ctrl Pts',(-16.95084263786,1.602157816061,-18.96518790099));
#19160=CARTESIAN_POINT('Ctrl Pts',(-16.44881838131,2.215365528923,-16.83088989051));
#19161=CARTESIAN_POINT('Ctrl Pts',(-16.44881838131,1.736642688769,-17.38740909059));
#19162=CARTESIAN_POINT('Ctrl Pts',(-16.44881838131,1.257919848614,-17.94392829068));
#19163=CARTESIAN_POINT('Ctrl Pts',(-16.44881838131,0.7791970084599,-18.50044749077));
#19164=CARTESIAN_POINT('Ctrl Pts',(-15.99393964446,2.105376743577,-16.6924369233));
#19165=CARTESIAN_POINT('Ctrl Pts',(-15.99393964446,1.441665263409,-17.01609396359));
#19166=CARTESIAN_POINT('Ctrl Pts',(-15.99393964446,0.7779537832405,-17.33975100388));
#19167=CARTESIAN_POINT('Ctrl Pts',(-15.99393964446,0.114242303072,-17.66340804417));
#19168=CARTESIAN_POINT('Ctrl Pts',(-15.71573553238,2.072985342811,-16.56136590274));
#19169=CARTESIAN_POINT('Ctrl Pts',(-15.71573553238,1.354795206866,-16.66457637875));
#19170=CARTESIAN_POINT('Ctrl Pts',(-15.71573553238,0.6366050709221,-16.76778685476));
#19171=CARTESIAN_POINT('Ctrl Pts',(-15.71573553238,-0.08158506502212,-16.87099733077));
#19172=CARTESIAN_POINT('Ctrl Pts',(-15.58265688292,2.074224564534,-16.49022669701));
#19173=CARTESIAN_POINT('Ctrl Pts',(-15.58265688292,1.358118658728,-16.47378911183));
#19174=CARTESIAN_POINT('Ctrl Pts',(-15.58265688292,0.6420127529222,-16.45735152665));
#19175=CARTESIAN_POINT('Ctrl Pts',(-15.58265688292,-0.07409315288371,-16.44091394148));
#19176=CARTESIAN_POINT('Ctrl Pts',(-15.5735533349,2.07439713734,-16.48531913027));
#19177=CARTESIAN_POINT('Ctrl Pts',(-15.5735533349,1.358581479386,-16.46062757543));
#19178=CARTESIAN_POINT('Ctrl Pts',(-15.5735533349,0.6427658214313,-16.43593602058));
#19179=CARTESIAN_POINT('Ctrl Pts',(-15.5735533349,-0.07304983652298,-16.41124446574));
#19180=CARTESIAN_POINT('',(-17.4999999999994,2.38270534092991,-18.9972468766531));
#19181=CARTESIAN_POINT('',(-17.4999999999987,2.42961219547651,-17.9985825134353));
#19182=CARTESIAN_POINT('Ctrl Pts',(-15.6010205144307,1.25767452008319E-15,
-16.5000000000003));
#19183=CARTESIAN_POINT('Ctrl Pts',(-15.6579985049851,2.17455779774946E-14,
-16.6772339549203));
#19184=CARTESIAN_POINT('Ctrl Pts',(-15.7175892974837,0.0188486066689643,
-16.8530406318105));
#19185=CARTESIAN_POINT('Ctrl Pts',(-15.841088915592,0.0914580806764069,
-17.1914308410855));
#19186=CARTESIAN_POINT('Ctrl Pts',(-15.9044838682972,0.144072067619024,
-17.3532507311179));
#19187=CARTESIAN_POINT('Ctrl Pts',(-16.0985790100571,0.342122917384096,
-17.8029799327834));
#19188=CARTESIAN_POINT('Ctrl Pts',(-16.2356039725905,0.526266781326162,
-18.0659091363647));
#19189=CARTESIAN_POINT('Ctrl Pts',(-16.5490224816406,0.990195424858404,
-18.5209523776298));
#19190=CARTESIAN_POINT('Ctrl Pts',(-16.7244456612409,1.27033612063607,-18.6999333325823));
#19191=CARTESIAN_POINT('Ctrl Pts',(-17.0103210025318,1.70441228965547,-18.8747029432739));
#19192=CARTESIAN_POINT('Ctrl Pts',(-17.1050393851134,1.8447164026833,-18.9168433193197));
#19193=CARTESIAN_POINT('Ctrl Pts',(-17.2988175722228,2.11884247458825,-18.974560464731));
#19194=CARTESIAN_POINT('Ctrl Pts',(-17.3971035117738,2.25218259631596,-18.9911162770022));
#19195=CARTESIAN_POINT('Ctrl Pts',(-17.4999999999985,2.38270534093059,-18.9972468766531));
#19196=CARTESIAN_POINT('Origin',(14.5,2.5,-17.));
#19197=CARTESIAN_POINT('',(-21.5,7.3,-17.));
#19198=CARTESIAN_POINT('',(-19.5,9.3,-17.));
#19199=CARTESIAN_POINT('Origin',(-19.5,7.3,-17.));
#19200=CARTESIAN_POINT('',(-21.5,5.910754259309,-17.));
#19201=CARTESIAN_POINT('',(-21.5,5.9,-17.));
#19202=CARTESIAN_POINT('',(-20.4999999999993,4.17870345173968,-17.));
#19203=CARTESIAN_POINT('Origin',(-19.5,5.910754259309,-17.));
#19204=CARTESIAN_POINT('',(-17.59240033074,2.5,-17.));
#19205=CARTESIAN_POINT('',(12.5,9.3,-17.));
#19206=CARTESIAN_POINT('Origin',(12.5,7.3,-17.));
#19207=CARTESIAN_POINT('',(14.5,9.3,-17.));
#19208=CARTESIAN_POINT('Origin',(14.5,2.5,16.5));
#19209=CARTESIAN_POINT('',(-17.5924003307403,2.4999999999995,19.));
#19210=CARTESIAN_POINT('',(14.5,2.5,19.));
#19211=CARTESIAN_POINT('Origin',(-17.546200165371,2.53637972596203,14.9500703324677));
#19212=CARTESIAN_POINT('Origin',(14.5,2.5,-16.5));
#19213=CARTESIAN_POINT('',(-17.5924003307402,2.49999999999858,-19.));
#19214=CARTESIAN_POINT('Origin',(-17.5462001653617,2.5363797259711,-14.9500703323505));
#19215=CARTESIAN_POINT('',(14.5,2.5,-19.));
#19216=CARTESIAN_POINT('Origin',(-19.54620016537,3.628026860465,18.));
#19217=CARTESIAN_POINT('',(-20.4999999999993,4.17870345174128,19.));
#19218=CARTESIAN_POINT('',(-19.54620016537,3.628026860465,19.));
#19219=CARTESIAN_POINT('',(-20.4999999999993,4.17870345174126,18.));
#19220=CARTESIAN_POINT('',(-17.5924003307406,2.49999999999901,17.6366197724371));
#19221=CARTESIAN_POINT('',(-17.5924003307406,2.49999999999901,18.));
#19222=CARTESIAN_POINT('',(-17.5924003307406,2.49999999999901,18.));
#19223=CARTESIAN_POINT('Origin',(-19.5,5.910754259309,16.91739728962));
#19224=CARTESIAN_POINT('',(-21.5,5.910754259309,19.));
#19225=CARTESIAN_POINT('Origin',(-19.5,5.910754259309,19.));
#19226=CARTESIAN_POINT('',(-21.5,5.910754259309,16.91739728962));
#19227=CARTESIAN_POINT('Origin',(-19.5,7.3,16.91739728962));
#19228=CARTESIAN_POINT('',(-21.5,7.3,19.));
#19229=CARTESIAN_POINT('',(-21.5,7.3,16.91739728962));
#19230=CARTESIAN_POINT('',(-19.5,9.3,19.));
#19231=CARTESIAN_POINT('Origin',(-19.5,7.3,19.));
#19232=CARTESIAN_POINT('',(-19.5,9.3,16.91739728962));
#19233=CARTESIAN_POINT('Origin',(-3.5,9.3,18.));
#19234=CARTESIAN_POINT('',(12.5,9.3,19.));
#19235=CARTESIAN_POINT('',(-3.5,9.3,19.));
#19236=CARTESIAN_POINT('',(12.5,9.3,18.));
#19237=CARTESIAN_POINT('Origin',(12.5,7.3,16.91739728962));
#19238=CARTESIAN_POINT('Origin',(12.5,7.3,19.));
#19239=CARTESIAN_POINT('Ctrl Pts',(-17.42814205157,2.464509271523,16.92437907463));
#19240=CARTESIAN_POINT('Ctrl Pts',(-17.42814205157,2.404830934618,17.63798058348));
#19241=CARTESIAN_POINT('Ctrl Pts',(-17.42814205157,2.345152597712,18.35158209233));
#19242=CARTESIAN_POINT('Ctrl Pts',(-17.42814205157,2.285474260807,19.06518360117));
#19243=CARTESIAN_POINT('Ctrl Pts',(-17.45209470105,2.469672618979,16.92481104223));
#19244=CARTESIAN_POINT('Ctrl Pts',(-17.45209470105,2.418676549309,17.63913891283));
#19245=CARTESIAN_POINT('Ctrl Pts',(-17.45209470105,2.367680479639,18.35346678343));
#19246=CARTESIAN_POINT('Ctrl Pts',(-17.45209470105,2.316684409969,19.06779465403));
#19247=CARTESIAN_POINT('Ctrl Pts',(-17.50684746077,2.481493415089,16.92558269389));
#19248=CARTESIAN_POINT('Ctrl Pts',(-17.50684746077,2.450374239556,17.64120811149));
#19249=CARTESIAN_POINT('Ctrl Pts',(-17.50684746077,2.419255064023,18.35683352909));
#19250=CARTESIAN_POINT('Ctrl Pts',(-17.50684746077,2.38813588849,19.07245894669));
#19251=CARTESIAN_POINT('Ctrl Pts',(-17.58555286997,2.498518773752,16.92598231066));
#19252=CARTESIAN_POINT('Ctrl Pts',(-17.58555286997,2.496028063562,17.64227969147));
#19253=CARTESIAN_POINT('Ctrl Pts',(-17.58555286997,2.493537353372,18.35857707229));
#19254=CARTESIAN_POINT('Ctrl Pts',(-17.58555286997,2.491046643181,19.0748744531));
#19255=CARTESIAN_POINT('Ctrl Pts',(-17.6403056297,2.510362756466,16.92576611527));
#19256=CARTESIAN_POINT('Ctrl Pts',(-17.6403056297,2.527787929129,17.64169995942));
#19257=CARTESIAN_POINT('Ctrl Pts',(-17.6403056297,2.545213101792,18.35763380357));
#19258=CARTESIAN_POINT('Ctrl Pts',(-17.6403056297,2.562638274455,19.07356764772));
#19259=CARTESIAN_POINT('Ctrl Pts',(-17.66425827917,2.515540684786,16.92557687661));
#19260=CARTESIAN_POINT('Ctrl Pts',(-17.66425827917,2.541672642685,17.64119251234));
#19261=CARTESIAN_POINT('Ctrl Pts',(-17.66425827917,2.567804600584,18.35680814807));
#19262=CARTESIAN_POINT('Ctrl Pts',(-17.66425827917,2.593936558484,19.0724237838));
#19263=CARTESIAN_POINT('Ctrl Pts',(-17.42814205157,2.464509271523,-16.92437907463));
#19264=CARTESIAN_POINT('Ctrl Pts',(-17.42814205157,2.404830934618,-17.63798058348));
#19265=CARTESIAN_POINT('Ctrl Pts',(-17.42814205157,2.345152597712,-18.35158209233));
#19266=CARTESIAN_POINT('Ctrl Pts',(-17.42814205157,2.285474260807,-19.06518360117));
#19267=CARTESIAN_POINT('Ctrl Pts',(-17.45209470105,2.469672618979,-16.92481104223));
#19268=CARTESIAN_POINT('Ctrl Pts',(-17.45209470105,2.418676549309,-17.63913891283));
#19269=CARTESIAN_POINT('Ctrl Pts',(-17.45209470105,2.367680479639,-18.35346678343));
#19270=CARTESIAN_POINT('Ctrl Pts',(-17.45209470105,2.316684409969,-19.06779465403));
#19271=CARTESIAN_POINT('Ctrl Pts',(-17.50684746077,2.481493415089,-16.92558269389));
#19272=CARTESIAN_POINT('Ctrl Pts',(-17.50684746077,2.450374239556,-17.64120811149));
#19273=CARTESIAN_POINT('Ctrl Pts',(-17.50684746077,2.419255064023,-18.35683352909));
#19274=CARTESIAN_POINT('Ctrl Pts',(-17.50684746077,2.38813588849,-19.07245894669));
#19275=CARTESIAN_POINT('Ctrl Pts',(-17.58555286997,2.498518773752,-16.92598231066));
#19276=CARTESIAN_POINT('Ctrl Pts',(-17.58555286997,2.496028063562,-17.64227969147));
#19277=CARTESIAN_POINT('Ctrl Pts',(-17.58555286997,2.493537353372,-18.35857707229));
#19278=CARTESIAN_POINT('Ctrl Pts',(-17.58555286997,2.491046643181,-19.0748744531));
#19279=CARTESIAN_POINT('Ctrl Pts',(-17.6403056297,2.510362756466,-16.92576611527));
#19280=CARTESIAN_POINT('Ctrl Pts',(-17.6403056297,2.527787929129,-17.64169995942));
#19281=CARTESIAN_POINT('Ctrl Pts',(-17.6403056297,2.545213101792,-18.35763380357));
#19282=CARTESIAN_POINT('Ctrl Pts',(-17.6403056297,2.562638274455,-19.07356764772));
#19283=CARTESIAN_POINT('Ctrl Pts',(-17.66425827917,2.515540684786,-16.92557687661));
#19284=CARTESIAN_POINT('Ctrl Pts',(-17.66425827917,2.541672642685,-17.64119251234));
#19285=CARTESIAN_POINT('Ctrl Pts',(-17.66425827917,2.567804600584,-18.35680814807));
#19286=CARTESIAN_POINT('Ctrl Pts',(-17.66425827917,2.593936558484,-19.0724237838));
#19287=CARTESIAN_POINT('',(-17.5924003307402,2.49999999999784,-17.636619772437));
#19288=CARTESIAN_POINT('',(-17.5924003307402,2.49999999999716,-18.0000000145074));
#19289=CARTESIAN_POINT('',(-17.5924003307402,2.49999999999716,-18.0000000145074));
#19290=CARTESIAN_POINT('Origin',(-3.5,9.3,-18.));
#19291=CARTESIAN_POINT('',(-19.5,9.3,-19.));
#19292=CARTESIAN_POINT('',(-19.5,9.3,-18.));
#19293=CARTESIAN_POINT('',(12.5,9.3,-19.));
#19294=CARTESIAN_POINT('',(12.5,9.3,-18.));
#19295=CARTESIAN_POINT('',(-3.5,9.3,-19.));
#19296=CARTESIAN_POINT('Origin',(-19.5,7.3,-16.91739728962));
#19297=CARTESIAN_POINT('',(-21.5,7.3,-19.));
#19298=CARTESIAN_POINT('Origin',(-19.5,7.3,-19.));
#19299=CARTESIAN_POINT('',(-21.5,7.3,-16.91739728962));
#19300=CARTESIAN_POINT('Origin',(-19.5,5.910754259309,-16.91739728962));
#19301=CARTESIAN_POINT('',(-21.5,5.910754259309,-19.));
#19302=CARTESIAN_POINT('',(-21.5,5.910754259309,-16.91739728962));
#19303=CARTESIAN_POINT('',(-20.4999999999997,4.1787034517407,-19.));
#19304=CARTESIAN_POINT('Origin',(-19.5,5.910754259309,-19.));
#19305=CARTESIAN_POINT('',(-20.5,4.17870345174009,-16.91739728962));
#19306=CARTESIAN_POINT('Origin',(-19.54620016537,3.628026860465,-18.));
#19307=CARTESIAN_POINT('',(-19.54620016537,3.628026860465,-19.));
#19308=CARTESIAN_POINT('Origin',(12.5,7.3,-16.91739728962));
#19309=CARTESIAN_POINT('Origin',(12.5,7.3,-19.));
#19310=CARTESIAN_POINT('Origin',(14.5,9.3,19.));
#19311=CARTESIAN_POINT('',(-21.5,9.3,19.));
#19312=CARTESIAN_POINT('Origin',(14.5,2.5,-19.));
#19313=CARTESIAN_POINT('',(-21.5,2.5,-19.));
#19314=CARTESIAN_POINT('Origin',(-21.5,5.9,18.));
#19315=CARTESIAN_POINT('Origin',(-21.5,5.9,-18.));
#19316=CARTESIAN_POINT('Origin',(8.,10.74803620541,-3.5));
#19317=CARTESIAN_POINT('',(8.,0.1,-2.25));
#19318=CARTESIAN_POINT('Origin',(8.,0.0999999999999994,-3.5));
#19319=CARTESIAN_POINT('',(8.,2.,-2.25));
#19320=CARTESIAN_POINT('',(8.,10.74803620541,-2.25));
#19321=CARTESIAN_POINT('Origin',(8.,2.,-3.5));
#19322=CARTESIAN_POINT('Origin',(3.5,10.74803620541,8.));
#19323=CARTESIAN_POINT('',(3.5,0.1,9.25));
#19324=CARTESIAN_POINT('Origin',(3.5,0.0999999999999994,8.));
#19325=CARTESIAN_POINT('',(3.5,2.,9.25));
#19326=CARTESIAN_POINT('',(3.5,10.74803620541,9.25));
#19327=CARTESIAN_POINT('Origin',(3.5,2.,8.));
#19328=CARTESIAN_POINT('Origin',(-8.,10.74803620541,3.5));
#19329=CARTESIAN_POINT('',(-8.,0.1,4.75));
#19330=CARTESIAN_POINT('Origin',(-8.,0.0999999999999994,3.5));
#19331=CARTESIAN_POINT('',(-8.,2.,4.75));
#19332=CARTESIAN_POINT('',(-8.,10.74803620541,4.75));
#19333=CARTESIAN_POINT('Origin',(-8.,2.,3.5));
#19334=CARTESIAN_POINT('Origin',(-3.5,10.74803620541,-8.));
#19335=CARTESIAN_POINT('',(-3.5,0.1,-6.75));
#19336=CARTESIAN_POINT('Origin',(-3.5,0.0999999999999994,-8.));
#19337=CARTESIAN_POINT('',(-3.5,2.,-6.75));
#19338=CARTESIAN_POINT('',(-3.5,10.74803620541,-6.75));
#19339=CARTESIAN_POINT('Origin',(-3.5,2.,-8.));
#19340=CARTESIAN_POINT('Origin',(6.,10.74803620541,-11.));
#19341=CARTESIAN_POINT('',(6.,0.1,-9.75));
#19342=CARTESIAN_POINT('Origin',(6.,0.0999999999999994,-11.));
#19343=CARTESIAN_POINT('',(6.,2.,-9.75));
#19344=CARTESIAN_POINT('',(6.,10.74803620541,-9.75));
#19345=CARTESIAN_POINT('Origin',(6.,2.,-11.));
#19346=CARTESIAN_POINT('Origin',(11.,10.74803620541,6.));
#19347=CARTESIAN_POINT('',(11.,0.1,7.25));
#19348=CARTESIAN_POINT('Origin',(11.,0.0999999999999994,6.));
#19349=CARTESIAN_POINT('',(11.,2.,7.25));
#19350=CARTESIAN_POINT('',(11.,10.74803620541,7.25));
#19351=CARTESIAN_POINT('Origin',(11.,2.,6.));
#19352=CARTESIAN_POINT('Origin',(-6.,10.74803620541,11.));
#19353=CARTESIAN_POINT('',(-6.,0.1,12.25));
#19354=CARTESIAN_POINT('Origin',(-6.,0.0999999999999994,11.));
#19355=CARTESIAN_POINT('',(-6.,2.,12.25));
#19356=CARTESIAN_POINT('',(-6.,10.74803620541,12.25));
#19357=CARTESIAN_POINT('Origin',(-6.,2.,11.));
#19358=CARTESIAN_POINT('Origin',(-11.,10.74803620541,-6.));
#19359=CARTESIAN_POINT('',(-11.,0.1,-4.75));
#19360=CARTESIAN_POINT('Origin',(-11.,0.0999999999999994,-6.));
#19361=CARTESIAN_POINT('',(-11.,2.,-4.75));
#19362=CARTESIAN_POINT('',(-11.,10.74803620541,-4.75));
#19363=CARTESIAN_POINT('Origin',(-11.,2.,-6.));
#19364=CARTESIAN_POINT('',(0.,0.,0.));
#19365=CARTESIAN_POINT('Origin',(0.,5.,-40.));
#19366=CARTESIAN_POINT('',(3.06161699786838E-16,2.91,-37.5));
#19367=CARTESIAN_POINT('',(-3.06161699786838E-16,2.91,-42.5));
#19368=CARTESIAN_POINT('Origin',(0.,2.91,-40.));
#19369=CARTESIAN_POINT('',(-5.62112880808636E-16,5.,-44.59));
#19370=CARTESIAN_POINT('',(-5.62112880808636E-16,5.,-44.59));
#19371=CARTESIAN_POINT('Origin',(0.,5.,-40.));
#19372=CARTESIAN_POINT('Origin',(0.,2.91,-40.));
#19373=CARTESIAN_POINT('Origin',(-7.77817459305202,0.,-7.77817459305202));
#19374=CARTESIAN_POINT('',(-7.77817459305202,0.,-9.02817459305202));
#19375=CARTESIAN_POINT('Origin',(-7.77817459305202,0.,-7.77817459305202));
#19376=CARTESIAN_POINT('',(-7.77817459305202,5.,-9.02817459305202));
#19377=CARTESIAN_POINT('',(-7.77817459305202,0.,-9.02817459305202));
#19378=CARTESIAN_POINT('Origin',(-7.77817459305202,5.,-7.77817459305202));
#19379=CARTESIAN_POINT('Origin',(-11.,0.,2.05998412772246E-15));
#19380=CARTESIAN_POINT('',(-11.,0.,-1.25));
#19381=CARTESIAN_POINT('Origin',(-11.,0.,2.05998412772246E-15));
#19382=CARTESIAN_POINT('',(-11.,5.,-1.25));
#19383=CARTESIAN_POINT('',(-11.,0.,-1.25));
#19384=CARTESIAN_POINT('Origin',(-11.,5.,2.05998412772246E-15));
#19385=CARTESIAN_POINT('Origin',(-7.77817459305202,0.,7.77817459305202));
#19386=CARTESIAN_POINT('',(-7.77817459305202,0.,6.52817459305202));
#19387=CARTESIAN_POINT('Origin',(-7.77817459305202,0.,7.77817459305202));
#19388=CARTESIAN_POINT('',(-7.77817459305202,5.,6.52817459305202));
#19389=CARTESIAN_POINT('',(-7.77817459305202,0.,6.52817459305202));
#19390=CARTESIAN_POINT('Origin',(-7.77817459305202,5.,7.77817459305202));
#19391=CARTESIAN_POINT('Origin',(1.30104260698261E-15,0.,11.));
#19392=CARTESIAN_POINT('',(1.14796175708919E-15,0.,9.75));
#19393=CARTESIAN_POINT('Origin',(1.30104260698261E-15,0.,11.));
#19394=CARTESIAN_POINT('',(1.14796175708919E-15,5.,9.75));
#19395=CARTESIAN_POINT('',(1.14796175708919E-15,0.,9.75));
#19396=CARTESIAN_POINT('Origin',(1.30104260698261E-15,5.,11.));
#19397=CARTESIAN_POINT('Origin',(7.77817459305202,0.,7.77817459305202));
#19398=CARTESIAN_POINT('',(7.77817459305202,0.,6.52817459305202));
#19399=CARTESIAN_POINT('Origin',(7.77817459305202,0.,7.77817459305202));
#19400=CARTESIAN_POINT('',(7.77817459305202,5.,6.52817459305202));
#19401=CARTESIAN_POINT('',(7.77817459305202,0.,6.52817459305202));
#19402=CARTESIAN_POINT('Origin',(7.77817459305202,5.,7.77817459305202));
#19403=CARTESIAN_POINT('Origin',(11.,0.,-8.67361737988404E-16));
#19404=CARTESIAN_POINT('',(11.,0.,-1.25));
#19405=CARTESIAN_POINT('Origin',(11.,0.,-8.67361737988404E-16));
#19406=CARTESIAN_POINT('',(11.,5.,-1.25));
#19407=CARTESIAN_POINT('',(11.,0.,-1.25));
#19408=CARTESIAN_POINT('Origin',(11.,5.,-8.67361737988404E-16));
#19409=CARTESIAN_POINT('Origin',(7.77817459305202,0.,-7.77817459305202));
#19410=CARTESIAN_POINT('',(7.77817459305202,0.,-9.02817459305203));
#19411=CARTESIAN_POINT('Origin',(7.77817459305202,0.,-7.77817459305202));
#19412=CARTESIAN_POINT('',(7.77817459305202,5.,-9.02817459305203));
#19413=CARTESIAN_POINT('',(7.77817459305202,0.,-9.02817459305203));
#19414=CARTESIAN_POINT('Origin',(7.77817459305202,5.,-7.77817459305202));
#19415=CARTESIAN_POINT('Origin',(0.,0.,-11.));
#19416=CARTESIAN_POINT('',(-1.53080849893419E-16,0.,-12.25));
#19417=CARTESIAN_POINT('Origin',(0.,0.,-11.));
#19418=CARTESIAN_POINT('',(-1.53080849893419E-16,5.,-12.25));
#19419=CARTESIAN_POINT('',(-1.53080849893419E-16,0.,-12.25));
#19420=CARTESIAN_POINT('Origin',(0.,5.,-11.));
#19421=CARTESIAN_POINT('Origin',(0.,5.,0.));
#19422=CARTESIAN_POINT('',(-6.73555739531044E-16,5.,5.5));
#19423=CARTESIAN_POINT('Origin',(0.,5.,0.));
#19424=CARTESIAN_POINT('',(-6.73555739531044E-16,0.,5.5));
#19425=CARTESIAN_POINT('',(-6.73555739531044E-16,5.,5.5));
#19426=CARTESIAN_POINT('Origin',(0.,0.,0.));
#19427=CARTESIAN_POINT('Origin',(0.,5.,-40.));
#19428=CARTESIAN_POINT('',(-3.06161699786839E-16,0.,-37.5));
#19429=CARTESIAN_POINT('',(-3.06161699786839E-16,5.,-37.5));
#19430=CARTESIAN_POINT('Origin',(0.,0.,-40.));
#19431=CARTESIAN_POINT('Origin',(0.,5.,0.));
#19432=CARTESIAN_POINT('',(-14.,5.,0.));
#19433=CARTESIAN_POINT('',(-8.9323613883135,5.,-41.1013264859097));
#19434=CARTESIAN_POINT('',(-13.7903595012355,5.,-1.70029933952269));
#19435=CARTESIAN_POINT('',(14.,5.,0.));
#19436=CARTESIAN_POINT('Origin',(0.,5.,0.));
#19437=CARTESIAN_POINT('',(8.9323613883135,5.,-41.1013264859097));
#19438=CARTESIAN_POINT('',(13.7903595012355,5.,-1.70029933952269));
#19439=CARTESIAN_POINT('Origin',(0.,5.,-40.));
#19440=CARTESIAN_POINT('Origin',(0.,0.,0.));
#19441=CARTESIAN_POINT('',(-14.,0.,0.));
#19442=CARTESIAN_POINT('',(14.,0.,0.));
#19443=CARTESIAN_POINT('Origin',(0.,0.,0.));
#19444=CARTESIAN_POINT('',(-8.9323613883135,0.,-41.1013264859097));
#19445=CARTESIAN_POINT('',(-13.7903595012355,0.,-1.70029933952269));
#19446=CARTESIAN_POINT('',(8.9323613883135,0.,-41.1013264859097));
#19447=CARTESIAN_POINT('Origin',(0.,0.,-40.));
#19448=CARTESIAN_POINT('',(13.7903595012355,0.,-1.70029933952269));
#19449=CARTESIAN_POINT('Origin',(0.,5.,0.));
#19450=CARTESIAN_POINT('',(14.,5.,0.));
#19451=CARTESIAN_POINT('',(-14.,5.,0.));
#19452=CARTESIAN_POINT('Origin',(0.,0.,-40.));
#19453=CARTESIAN_POINT('',(8.9323613883135,0.,-41.1013264859097));
#19454=CARTESIAN_POINT('',(-8.9323613883135,0.,-41.1013264859097));
#19455=CARTESIAN_POINT('Origin',(-13.7903595012355,0.,-1.70029933952269));
#19456=CARTESIAN_POINT('Origin',(13.7903595012355,0.,-1.70029933952269));
#19457=CARTESIAN_POINT('',(0.,0.,0.));
#19458=CARTESIAN_POINT('',(0.,0.,0.));
#19459=CARTESIAN_POINT('Origin',(-38.001,20.,-48.));
#19460=CARTESIAN_POINT('',(-6.,20.,-35.5));
#19461=CARTESIAN_POINT('Origin',(-6.,20.,-48.));
#19462=CARTESIAN_POINT('',(0.,20.,-35.5));
#19463=CARTESIAN_POINT('',(-38.001,20.,-35.5));
#19464=CARTESIAN_POINT('Origin',(0.,20.,-48.));
#19465=CARTESIAN_POINT('Origin',(-38.001,20.,-118.));
#19466=CARTESIAN_POINT('',(-6.,20.,-105.5));
#19467=CARTESIAN_POINT('Origin',(-6.,20.,-118.));
#19468=CARTESIAN_POINT('',(0.,20.,-105.5));
#19469=CARTESIAN_POINT('',(-38.001,20.,-105.5));
#19470=CARTESIAN_POINT('Origin',(0.,20.,-118.));
#19471=CARTESIAN_POINT('Origin',(-38.001,20.,-83.));
#19472=CARTESIAN_POINT('',(-6.,20.,-70.5));
#19473=CARTESIAN_POINT('Origin',(-6.,20.,-83.));
#19474=CARTESIAN_POINT('',(0.,20.,-70.5));
#19475=CARTESIAN_POINT('',(-38.001,20.,-70.5));
#19476=CARTESIAN_POINT('Origin',(0.,20.,-83.));
#19477=CARTESIAN_POINT('Origin',(12.,-6.93889390390723E-15,3.46944695195361E-15));
#19478=CARTESIAN_POINT('',(1.31131748603704,10.,5.45454545454546));
#19479=CARTESIAN_POINT('',(12.,10.,-12.));
#19480=CARTESIAN_POINT('Origin',(12.,10.,3.46944695195361E-15));
#19481=CARTESIAN_POINT('',(12.,30.,-12.));
#19482=CARTESIAN_POINT('',(12.,-0.00100000000000794,-12.));
#19483=CARTESIAN_POINT('',(1.31131748603704,30.,5.45454545454546));
#19484=CARTESIAN_POINT('Origin',(12.,30.,3.46944695195361E-15));
#19485=CARTESIAN_POINT('',(1.31131748603704,-6.93889390390723E-15,5.45454545454546));
#19486=CARTESIAN_POINT('Origin',(12.,-6.93889390390723E-15,3.46944695195361E-15));
#19487=CARTESIAN_POINT('',(12.,10.,-8.));
#19488=CARTESIAN_POINT('Origin',(12.,10.,3.46944695195361E-15));
#19489=CARTESIAN_POINT('',(12.,30.,-8.));
#19490=CARTESIAN_POINT('',(12.,-6.93889390390723E-15,-8.));
#19491=CARTESIAN_POINT('Origin',(12.,30.,3.46944695195361E-15));
#19492=CARTESIAN_POINT('Origin',(-26.,40.,-12.));
#19493=CARTESIAN_POINT('',(-26.,30.,-4.));
#19494=CARTESIAN_POINT('Origin',(-26.,30.,-12.));
#19495=CARTESIAN_POINT('',(-26.,10.,-4.));
#19496=CARTESIAN_POINT('',(-26.,40.,-4.));
#19497=CARTESIAN_POINT('Origin',(-26.,10.,-12.));
#19498=CARTESIAN_POINT('Origin',(0.,40.,0.));
#19499=CARTESIAN_POINT('',(0.,30.,1.73472347597681E-15));
#19500=CARTESIAN_POINT('',(0.,30.,-22.));
#19501=CARTESIAN_POINT('',(-1.24683249835833E-15,30.,12.001));
#19502=CARTESIAN_POINT('',(4.87890977618477E-16,10.,-22.));
#19503=CARTESIAN_POINT('',(0.,10.,-22.));
#19504=CARTESIAN_POINT('',(3.46944695195361E-15,10.,1.73472347597681E-15));
#19505=CARTESIAN_POINT('',(4.87890977618477E-16,10.,12.001));
#19506=CARTESIAN_POINT('',(0.,0.,-10.));
#19507=CARTESIAN_POINT('',(0.,-1.22464679914735E-15,-10.));
#19508=CARTESIAN_POINT('',(0.,-6.93889390390723E-15,-134.));
#19509=CARTESIAN_POINT('',(0.,0.,0.));
#19510=CARTESIAN_POINT('',(0.,10.,-144.));
#19511=CARTESIAN_POINT('',(0.,10.,-144.));
#19512=CARTESIAN_POINT('',(0.,30.,-144.));
#19513=CARTESIAN_POINT('',(0.,40.,-144.));
#19514=CARTESIAN_POINT('',(0.,40.,-134.));
#19515=CARTESIAN_POINT('',(0.,40.,-134.));
#19516=CARTESIAN_POINT('',(0.,40.,-10.));
#19517=CARTESIAN_POINT('',(0.,40.,0.));
#19518=CARTESIAN_POINT('',(0.,30.,1.73472347597681E-15));
#19519=CARTESIAN_POINT('Origin',(-26.,40.,-12.));
#19520=CARTESIAN_POINT('',(-6.,40.,-10.));
#19521=CARTESIAN_POINT('',(24.001,40.,-10.));
#19522=CARTESIAN_POINT('',(-6.,40.,-134.));
#19523=CARTESIAN_POINT('',(-6.,40.,-134.));
#19524=CARTESIAN_POINT('',(-6.,40.,-24.));
#19525=CARTESIAN_POINT('Origin',(-26.,0.,-12.));
#19526=CARTESIAN_POINT('',(-6.,-1.22464679914735E-15,-10.));
#19527=CARTESIAN_POINT('',(24.001,-1.22464679914735E-15,-10.));
#19528=CARTESIAN_POINT('',(-6.,0.,-134.));
#19529=CARTESIAN_POINT('',(-6.,0.,-24.));
#19530=CARTESIAN_POINT('',(-26.,0.,-134.));
#19531=CARTESIAN_POINT('Origin',(0.,40.,0.));
#19532=CARTESIAN_POINT('',(-7.59591794226543,10.,2.37360262678768E-15));
#19533=CARTESIAN_POINT('',(-26.,10.,8.67361737988404E-15));
#19534=CARTESIAN_POINT('',(-6.,10.,1.73472347597681E-15));
#19535=CARTESIAN_POINT('',(-7.59591794226543,30.,3.27314145353471E-15));
#19536=CARTESIAN_POINT('',(-7.59591794226543,40.,3.04080396370184E-15));
#19537=CARTESIAN_POINT('',(-26.,30.,8.67361737988404E-15));
#19538=CARTESIAN_POINT('',(-6.,30.,1.73472347597681E-15));
#19539=CARTESIAN_POINT('',(-26.,40.,8.67361737988404E-15));
#19540=CARTESIAN_POINT('Origin',(0.,40.,-144.));
#19541=CARTESIAN_POINT('',(-6.,10.,-144.));
#19542=CARTESIAN_POINT('',(0.,10.,-144.));
#19543=CARTESIAN_POINT('',(-6.,30.,-144.));
#19544=CARTESIAN_POINT('',(-6.,40.,-144.));
#19545=CARTESIAN_POINT('',(0.,30.,-144.));
#19546=CARTESIAN_POINT('Origin',(-6.,40.,-24.));
#19547=CARTESIAN_POINT('',(-6.,10.,1.73472347597681E-15));
#19548=CARTESIAN_POINT('',(-6.,-1.22464679914735E-15,-10.));
#19549=CARTESIAN_POINT('',(-6.,10.,-34.));
#19550=CARTESIAN_POINT('',(-6.,10.,12.001));
#19551=CARTESIAN_POINT('',(-6.,30.,-34.));
#19552=CARTESIAN_POINT('',(-6.,30.,-34.));
#19553=CARTESIAN_POINT('',(-6.,30.,2.77555756156289E-15));
#19554=CARTESIAN_POINT('',(-6.,30.,12.001));
#19555=CARTESIAN_POINT('',(-6.,30.,1.73472347597681E-15));
#19556=CARTESIAN_POINT('',(-6.,40.,-134.));
#19557=CARTESIAN_POINT('',(-6.,10.,-144.));
#19558=CARTESIAN_POINT('Origin',(-6.,40.,-24.));
#19559=CARTESIAN_POINT('',(-16.,30.,-24.));
#19560=CARTESIAN_POINT('',(-26.,30.,-24.));
#19561=CARTESIAN_POINT('',(-6.,30.,-24.));
#19562=CARTESIAN_POINT('',(-16.,10.,-24.));
#19563=CARTESIAN_POINT('',(-16.,10.,-24.));
#19564=CARTESIAN_POINT('',(-26.,10.,-24.));
#19565=CARTESIAN_POINT('',(-6.,10.,-24.));
#19566=CARTESIAN_POINT('',(-26.,40.,-24.));
#19567=CARTESIAN_POINT('Origin',(-26.,40.,-12.));
#19568=CARTESIAN_POINT('Origin',(-26.,10.,-12.));
#19569=CARTESIAN_POINT('Origin',(-26.,30.,-12.));
#19570=CARTESIAN_POINT('Origin',(0.,10.,-144.));
#19571=CARTESIAN_POINT('Origin',(-26.,40.,-134.));
#19572=CARTESIAN_POINT('Origin',(-6.,30.,12.001));
#19573=CARTESIAN_POINT('Origin',(-7.59591794226543,30.,10.));
#19574=CARTESIAN_POINT('',(10.,30.,-12.));
#19575=CARTESIAN_POINT('',(12.,30.,-12.));
#19576=CARTESIAN_POINT('Origin',(10.,30.,-22.));
#19577=CARTESIAN_POINT('',(24.001,30.,-2.42878633871514E-15));
#19578=CARTESIAN_POINT('Origin',(-16.,30.,-34.));
#19579=CARTESIAN_POINT('Origin',(4.87890977618477E-16,10.,12.001));
#19580=CARTESIAN_POINT('',(10.,10.,-12.));
#19581=CARTESIAN_POINT('',(12.,10.,-12.));
#19582=CARTESIAN_POINT('Origin',(-7.59591794226543,10.,10.));
#19583=CARTESIAN_POINT('Origin',(-16.,10.,-34.));
#19584=CARTESIAN_POINT('',(-3.67579230942105E-15,10.,8.67361737988404E-15));
#19585=CARTESIAN_POINT('Origin',(10.,10.,-22.));
#19586=CARTESIAN_POINT('Origin',(-16.,40.,-34.));
#19587=CARTESIAN_POINT('Origin',(24.001,30.,1.73472347597681E-15));
#19588=CARTESIAN_POINT('Origin',(24.001,-1.22464679914735E-15,-10.));
#19589=CARTESIAN_POINT('Origin',(12.,-0.00100000000000794,-12.));
#19590=CARTESIAN_POINT('',(10.,30.,-12.));
#19591=CARTESIAN_POINT('Origin',(10.,-0.00100000000000794,-22.));
#19592=CARTESIAN_POINT('Origin',(-7.59591794226543,-6.93889390390723E-15,
10.));
#19593=CARTESIAN_POINT('',(0.,0.,0.));
#19594=CARTESIAN_POINT('Origin',(50.,20.,10.));
#19595=CARTESIAN_POINT('',(50.,-20.,0.));
#19596=CARTESIAN_POINT('',(50.,20.,0.));
#19597=CARTESIAN_POINT('',(50.,20.,0.));
#19598=CARTESIAN_POINT('',(50.,20.,10.));
#19599=CARTESIAN_POINT('',(50.,20.,10.));
#19600=CARTESIAN_POINT('',(50.,-20.,10.));
#19601=CARTESIAN_POINT('',(50.,20.,10.));
#19602=CARTESIAN_POINT('',(50.,-20.,10.));
#19603=CARTESIAN_POINT('Origin',(-50.,20.,10.));
#19604=CARTESIAN_POINT('',(-50.,20.,0.));
#19605=CARTESIAN_POINT('',(-50.,20.,0.));
#19606=CARTESIAN_POINT('',(-50.,20.,10.));
#19607=CARTESIAN_POINT('',(-50.,20.,10.));
#19608=CARTESIAN_POINT('',(-50.,20.,10.));
#19609=CARTESIAN_POINT('Origin',(-50.,20.,10.));
#19610=CARTESIAN_POINT('',(-50.,-20.,0.));
#19611=CARTESIAN_POINT('',(-50.,20.,0.));
#19612=CARTESIAN_POINT('',(-50.,-20.,10.));
#19613=CARTESIAN_POINT('',(-50.,-20.,10.));
#19614=CARTESIAN_POINT('',(-50.,20.,10.));
#19615=CARTESIAN_POINT('Origin',(-50.,-20.,10.));
#19616=CARTESIAN_POINT('',(-50.,-20.,0.));
#19617=CARTESIAN_POINT('',(-50.,-20.,10.));
#19618=CARTESIAN_POINT('Origin',(0.,0.,10.));
#19619=CARTESIAN_POINT('Origin',(0.,0.,0.));
#19620=CARTESIAN_POINT('',(0.,0.,0.));
#19621=CARTESIAN_POINT('',(0.,0.,0.));
#19622=CARTESIAN_POINT('Origin',(13.,-20.,19.5));
#19623=CARTESIAN_POINT('',(13.,-10.,11.5));
#19624=CARTESIAN_POINT('Origin',(13.,-10.,19.5));
#19625=CARTESIAN_POINT('',(13.,10.,11.5));
#19626=CARTESIAN_POINT('',(13.,-20.,11.5));
#19627=CARTESIAN_POINT('Origin',(13.,10.,19.5));
#19628=CARTESIAN_POINT('Origin',(-7.7,-20.,25.5));
#19629=CARTESIAN_POINT('',(-7.7,-20.,24.25));
#19630=CARTESIAN_POINT('Origin',(-7.7,-20.,25.5));
#19631=CARTESIAN_POINT('',(-7.7,-17.,24.25));
#19632=CARTESIAN_POINT('',(-7.7,-20.,24.25));
#19633=CARTESIAN_POINT('Origin',(-7.7,-17.,25.5));
#19634=CARTESIAN_POINT('Origin',(-7.7,-20.,25.5));
#19635=CARTESIAN_POINT('',(-7.7,17.,24.25));
#19636=CARTESIAN_POINT('Origin',(-7.7,17.,25.5));
#19637=CARTESIAN_POINT('',(-7.7,20.,24.25));
#19638=CARTESIAN_POINT('',(-7.7,-20.,24.25));
#19639=CARTESIAN_POINT('Origin',(-7.7,20.,25.5));
#19640=CARTESIAN_POINT('Origin',(-7.7,-20.,3.5));
#19641=CARTESIAN_POINT('',(-7.7,-20.,2.25));
#19642=CARTESIAN_POINT('Origin',(-7.7,-20.,3.5));
#19643=CARTESIAN_POINT('',(-7.7,-17.,2.25));
#19644=CARTESIAN_POINT('',(-7.7,-20.,2.25));
#19645=CARTESIAN_POINT('Origin',(-7.7,-17.,3.5));
#19646=CARTESIAN_POINT('Origin',(-7.7,-20.,3.5));
#19647=CARTESIAN_POINT('',(-7.7,17.,2.25));
#19648=CARTESIAN_POINT('Origin',(-7.7,17.,3.5));
#19649=CARTESIAN_POINT('',(-7.7,20.,2.25));
#19650=CARTESIAN_POINT('',(-7.7,-20.,2.25));
#19651=CARTESIAN_POINT('Origin',(-7.7,20.,3.5));
#19652=CARTESIAN_POINT('Origin',(-10.5,20.,36.));
#19653=CARTESIAN_POINT('',(-10.5,17.,33.));
#19654=CARTESIAN_POINT('',(-10.5,17.,3.00000000000001));
#19655=CARTESIAN_POINT('',(-10.5,17.,36.));
#19656=CARTESIAN_POINT('',(-10.5,20.,33.));
#19657=CARTESIAN_POINT('',(-10.5,20.,33.));
#19658=CARTESIAN_POINT('',(-10.5,20.,3.00000000000001));
#19659=CARTESIAN_POINT('',(-10.5,20.,36.));
#19660=CARTESIAN_POINT('',(-10.5,20.,3.));
#19661=CARTESIAN_POINT('Origin',(-10.5,17.,36.));
#19662=CARTESIAN_POINT('',(-7.5,17.,36.));
#19663=CARTESIAN_POINT('',(-3.,17.,36.));
#19664=CARTESIAN_POINT('',(-10.5,17.,36.));
#19665=CARTESIAN_POINT('',(-7.5,17.,36.));
#19666=CARTESIAN_POINT('',(-7.49999999999999,17.,0.));
#19667=CARTESIAN_POINT('',(-10.5,17.,3.));
#19668=CARTESIAN_POINT('',(-3.,17.,0.));
#19669=CARTESIAN_POINT('',(-10.5,17.,0.));
#19670=CARTESIAN_POINT('',(-3.,17.,36.));
#19671=CARTESIAN_POINT('Origin',(-3.,17.,36.));
#19672=CARTESIAN_POINT('',(-2.99999999999999,-17.,0.));
#19673=CARTESIAN_POINT('',(-3.,17.,0.));
#19674=CARTESIAN_POINT('',(-2.99999999999999,-17.,36.));
#19675=CARTESIAN_POINT('',(-2.99999999999999,-17.,36.));
#19676=CARTESIAN_POINT('',(-3.,17.,36.));
#19677=CARTESIAN_POINT('Origin',(-10.5,-17.,36.));
#19678=CARTESIAN_POINT('',(-10.5,-17.,33.));
#19679=CARTESIAN_POINT('',(-10.5,-17.,3.00000000000001));
#19680=CARTESIAN_POINT('',(-10.5,-17.,36.));
#19681=CARTESIAN_POINT('',(-7.5,-17.,36.));
#19682=CARTESIAN_POINT('',(-7.5,-17.,36.));
#19683=CARTESIAN_POINT('',(-10.5,-17.,36.));
#19684=CARTESIAN_POINT('',(-7.49999999999999,-17.,-2.16840434497101E-16));
#19685=CARTESIAN_POINT('',(-10.5,-17.,0.));
#19686=CARTESIAN_POINT('',(-10.5,-17.,3.));
#19687=CARTESIAN_POINT('Origin',(-10.5,-17.,36.));
#19688=CARTESIAN_POINT('',(-10.5,-20.,33.));
#19689=CARTESIAN_POINT('',(-10.5,-20.,3.00000000000001));
#19690=CARTESIAN_POINT('',(-10.5,-20.,36.));
#19691=CARTESIAN_POINT('',(-10.5,-17.,33.));
#19692=CARTESIAN_POINT('',(-10.5,-17.,3.));
#19693=CARTESIAN_POINT('Origin',(-10.5,-20.,36.));
#19694=CARTESIAN_POINT('',(-7.49999999999999,-20.,0.));
#19695=CARTESIAN_POINT('',(-2.,-20.,0.));
#19696=CARTESIAN_POINT('',(-10.5,-20.,0.));
#19697=CARTESIAN_POINT('',(-2.,-20.,36.));
#19698=CARTESIAN_POINT('',(-2.,-20.,36.));
#19699=CARTESIAN_POINT('',(-7.5,-20.,36.));
#19700=CARTESIAN_POINT('',(-10.5,-20.,36.));
#19701=CARTESIAN_POINT('',(-7.5,-20.,36.));
#19702=CARTESIAN_POINT('',(-10.5,-20.,3.));
#19703=CARTESIAN_POINT('Origin',(-10.5,20.,36.));
#19704=CARTESIAN_POINT('',(-2.00000000000001,20.,36.));
#19705=CARTESIAN_POINT('',(-7.5,20.,36.));
#19706=CARTESIAN_POINT('',(-10.5,20.,36.));
#19707=CARTESIAN_POINT('',(-2.00000000000001,20.,0.));
#19708=CARTESIAN_POINT('',(-2.00000000000001,20.,36.));
#19709=CARTESIAN_POINT('',(-7.49999999999999,20.,-2.16840434497101E-16));
#19710=CARTESIAN_POINT('',(-10.5,20.,0.));
#19711=CARTESIAN_POINT('',(-10.5,20.,3.));
#19712=CARTESIAN_POINT('',(-7.5,20.,36.));
#19713=CARTESIAN_POINT('Origin',(0.,0.,36.));
#19714=CARTESIAN_POINT('',(6.93889390390723E-15,-18.,36.));
#19715=CARTESIAN_POINT('',(8.99999999999999,-8.99999999999993,36.));
#19716=CARTESIAN_POINT('',(6.93889390390723E-15,-10.,36.));
#19717=CARTESIAN_POINT('',(6.93889390390723E-15,20.,36.));
#19718=CARTESIAN_POINT('',(1.22464679914735E-15,10.,36.));
#19719=CARTESIAN_POINT('',(6.93889390390723E-15,20.,36.));
#19720=CARTESIAN_POINT('',(5.50010745544284E-15,18.,36.));
#19721=CARTESIAN_POINT('',(6.93889390390723E-15,20.,36.));
#19722=CARTESIAN_POINT('',(9.,9.00000000000003,36.));
#19723=CARTESIAN_POINT('',(-7.5,17.,36.));
#19724=CARTESIAN_POINT('',(-7.5,-20.,36.));
#19725=CARTESIAN_POINT('Origin',(0.,0.,0.));
#19726=CARTESIAN_POINT('',(6.50521303491303E-15,-18.,0.));
#19727=CARTESIAN_POINT('',(1.22464679914735E-15,-10.,0.));
#19728=CARTESIAN_POINT('',(6.93889390390723E-15,20.,0.));
#19729=CARTESIAN_POINT('',(-2.,-20.,0.));
#19730=CARTESIAN_POINT('',(-7.49999999999999,0.,0.));
#19731=CARTESIAN_POINT('',(-7.49999999999999,0.,0.));
#19732=CARTESIAN_POINT('',(5.79604448295525E-15,18.,0.));
#19733=CARTESIAN_POINT('',(5.79604448295525E-15,18.,0.));
#19734=CARTESIAN_POINT('',(1.22464679914735E-15,10.,0.));
#19735=CARTESIAN_POINT('',(6.93889390390723E-15,20.,0.));
#19736=CARTESIAN_POINT('',(6.93889390390723E-15,20.,0.));
#19737=CARTESIAN_POINT('Origin',(-7.5,0.,36.));
#19738=CARTESIAN_POINT('Origin',(-10.5,-17.,3.));
#19739=CARTESIAN_POINT('Origin',(-7.5,0.,36.));
#19740=CARTESIAN_POINT('Origin',(-10.5,20.,3.));
#19741=CARTESIAN_POINT('Origin',(13.,-20.,19.5));
#19742=CARTESIAN_POINT('',(13.,-10.,7.5));
#19743=CARTESIAN_POINT('',(13.,-10.,31.5));
#19744=CARTESIAN_POINT('Origin',(13.,-10.,19.5));
#19745=CARTESIAN_POINT('',(13.,10.,7.5));
#19746=CARTESIAN_POINT('',(13.,-20.,7.5));
#19747=CARTESIAN_POINT('',(13.,10.,31.5));
#19748=CARTESIAN_POINT('Origin',(13.,10.,19.5));
#19749=CARTESIAN_POINT('',(13.,-20.,31.5));
#19750=CARTESIAN_POINT('Origin',(13.,-20.,31.5));
#19751=CARTESIAN_POINT('',(8.35164654424504,-10.,31.5));
#19752=CARTESIAN_POINT('',(13.,-10.,31.5));
#19753=CARTESIAN_POINT('',(8.35164654424504,10.,31.5));
#19754=CARTESIAN_POINT('',(13.,10.,31.5));
#19755=CARTESIAN_POINT('',(8.35164654424504,-20.,31.5));
#19756=CARTESIAN_POINT('Origin',(13.,-20.,7.5));
#19757=CARTESIAN_POINT('',(9.68245836551855,-10.,7.5));
#19758=CARTESIAN_POINT('',(13.,-10.,7.5));
#19759=CARTESIAN_POINT('',(9.68245836551855,10.,7.5));
#19760=CARTESIAN_POINT('',(9.68245836551855,20.,7.5));
#19761=CARTESIAN_POINT('',(13.,10.,7.5));
#19762=CARTESIAN_POINT('Origin',(9.68245836551855,20.,-2.5));
#19763=CARTESIAN_POINT('Origin',(9.68245836551855,-10.,-2.5));
#19764=CARTESIAN_POINT('Origin',(9.68245836551855,10.,-2.5));
#19765=CARTESIAN_POINT('Origin',(8.35164654424504,20.,41.5));
#19766=CARTESIAN_POINT('Origin',(8.35164654424504,-10.,41.5));
#19767=CARTESIAN_POINT('Origin',(8.35164654424504,10.,41.5));
#19768=CARTESIAN_POINT('Origin',(1.22464679914735E-15,10.,0.));
#19769=CARTESIAN_POINT('',(1.22464679914735E-15,10.,0.));
#19770=CARTESIAN_POINT('Origin',(6.93889390390723E-15,20.,0.));
#19771=CARTESIAN_POINT('',(5.79604448295525E-15,18.,0.));
#19772=CARTESIAN_POINT('Origin',(1.22464679914735E-15,-10.,0.));
#19773=CARTESIAN_POINT('',(1.22464679914735E-15,-10.,0.));
#19774=CARTESIAN_POINT('Origin',(6.93889390390723E-15,-20.,0.));
#19775=CARTESIAN_POINT('',(5.79604448295524E-15,-18.,0.));
#19776=CARTESIAN_POINT('Origin',(-2.,-20.,36.));
#19777=CARTESIAN_POINT('Origin',(5.79604448295525E-15,18.,0.));
#19778=CARTESIAN_POINT('',(0.,0.,0.));
#19779=CARTESIAN_POINT('Origin',(0.,0.,-3.46944695195361E-15));
#19780=CARTESIAN_POINT('',(-5.51648351648352,6.75574388101068E-16,1.11111111111111));
#19781=CARTESIAN_POINT('Origin',(0.,0.,1.11111111111111));
#19782=CARTESIAN_POINT('',(-5.51648351648352,-6.75574388101067E-16,-1.11111111111111));
#19783=CARTESIAN_POINT('Origin',(-6.,-7.34788079488412E-16,-3.46944695195361E-15));
#19784=CARTESIAN_POINT('Origin',(0.,0.,-1.11111111111111));
#19785=CARTESIAN_POINT('Origin',(0.,0.,2.5));
#19786=CARTESIAN_POINT('',(-4.,-4.89858719658941E-16,2.25));
#19787=CARTESIAN_POINT('Origin',(0.,0.,2.25));
#19788=CARTESIAN_POINT('',(-4.25,-5.20474889637625E-16,2.5));
#19789=CARTESIAN_POINT('',(-4.25,-5.20474889637625E-16,2.5));
#19790=CARTESIAN_POINT('Origin',(0.,0.,2.5));
#19791=CARTESIAN_POINT('Origin',(0.,0.,2.5));
#19792=CARTESIAN_POINT('',(4.,5.05166804648283E-16,-2.25));
#19793=CARTESIAN_POINT('',(-4.,-4.89858719658941E-16,-2.25));
#19794=CARTESIAN_POINT('Origin',(0.,0.,-2.25));
#19795=CARTESIAN_POINT('Origin',(0.,0.,-2.25));
#19796=CARTESIAN_POINT('',(-4.,-4.89858719658941E-16,2.5));
#19797=CARTESIAN_POINT('Origin',(0.,0.,-2.25));
#19798=CARTESIAN_POINT('',(4.25,-5.20474889637625E-16,-2.5));
#19799=CARTESIAN_POINT('',(4.,-4.89858719658941E-16,-2.25));
#19800=CARTESIAN_POINT('Origin',(0.,0.,-2.5));
#19801=CARTESIAN_POINT('Origin',(0.,0.,2.5));
#19802=CARTESIAN_POINT('',(-5.51648351648352,-6.75574388101067E-16,-2.5));
#19803=CARTESIAN_POINT('',(-5.51648351648352,-6.75574388101067E-16,2.5));
#19804=CARTESIAN_POINT('Origin',(0.,0.,-2.5));
#19805=CARTESIAN_POINT('Origin',(0.,0.,2.5));
#19806=CARTESIAN_POINT('',(-5.51648351648352,-6.75574388101067E-16,2.5));
#19807=CARTESIAN_POINT('Origin',(0.,0.,2.5));
#19808=CARTESIAN_POINT('',(-5.51648351648352,-6.75574388101067E-16,2.5));
#19809=CARTESIAN_POINT('Origin',(0.,5.51648351648352,2.5));
#19810=CARTESIAN_POINT('Origin',(0.,4.25,-2.5));
#19811=CARTESIAN_POINT('Origin',(0.,6.,0.));
#19812=CARTESIAN_POINT('',(-1.21175743903915,6.,9.08672536706121E-33));
#19813=CARTESIAN_POINT('',(1.21175743903915,6.,9.08672536706121E-33));
#19814=CARTESIAN_POINT('Origin',(0.,6.,0.));
#19815=CARTESIAN_POINT('Origin',(3.00000000000001,5.19615242270663,0.));
#19816=CARTESIAN_POINT('',(1.95058727456733,5.8020311422262,1.67904451446101E-32));
#19817=CARTESIAN_POINT('',(4.04941272543268,4.59027370318705,1.38300558951226E-33));
#19818=CARTESIAN_POINT('Origin',(3.00000000000001,5.19615242270663,0.));
#19819=CARTESIAN_POINT('Origin',(5.19615242270664,2.99999999999999,0.));
#19820=CARTESIAN_POINT('',(4.59027370318707,4.04941272543267,2.44941649221591E-32));
#19821=CARTESIAN_POINT('',(5.80203114222621,1.95058727456731,-6.32071418803668E-33));
#19822=CARTESIAN_POINT('Origin',(5.19615242270664,2.99999999999999,0.));
#19823=CARTESIAN_POINT('Origin',(6.,-2.08166817117217E-14,0.));
#19824=CARTESIAN_POINT('',(6.00000000000001,1.21175743903913,9.0867253670611E-33));
#19825=CARTESIAN_POINT('',(6.,-1.21175743903917,9.08672536706132E-33));
#19826=CARTESIAN_POINT('Origin',(6.,-2.08166817117217E-14,0.));
#19827=CARTESIAN_POINT('Origin',(5.19615242270662,-3.00000000000002,0.));
#19828=CARTESIAN_POINT('',(5.8020311422262,-1.95058727456735,-6.32071418803668E-33));
#19829=CARTESIAN_POINT('',(4.59027370318704,-4.0494127254327,2.44941649221591E-32));
#19830=CARTESIAN_POINT('Origin',(5.19615242270662,-3.00000000000002,0.));
#19831=CARTESIAN_POINT('Origin',(2.99999999999997,-5.19615242270665,0.));
#19832=CARTESIAN_POINT('',(4.04941272543265,-4.59027370318708,1.67904451446102E-32));
#19833=CARTESIAN_POINT('',(1.95058727456729,-5.80203114222622,1.38300558951227E-33));
#19834=CARTESIAN_POINT('Origin',(2.99999999999997,-5.19615242270665,0.));
#19835=CARTESIAN_POINT('Origin',(-4.16333634234434E-14,-6.,0.));
#19836=CARTESIAN_POINT('',(1.21175743903911,-6.00000000000001,9.08672536706099E-33));
#19837=CARTESIAN_POINT('',(-1.21175743903919,-5.99999999999999,9.08672536706142E-33));
#19838=CARTESIAN_POINT('Origin',(-4.16333634234434E-14,-6.,0.));
#19839=CARTESIAN_POINT('Origin',(-3.00000000000004,-5.19615242270661,0.));
#19840=CARTESIAN_POINT('',(-1.95058727456737,-5.80203114222619,3.2197884699708E-32));
#19841=CARTESIAN_POINT('',(-4.04941272543271,-4.59027370318703,-1.40244339655856E-32));
#19842=CARTESIAN_POINT('Origin',(-3.00000000000004,-5.19615242270661,0.));
#19843=CARTESIAN_POINT('Origin',(-5.19615242270666,-2.99999999999995,0.));
#19844=CARTESIAN_POINT('',(-4.5902737031871,-4.04941272543263,-6.32071418803668E-33));
#19845=CARTESIAN_POINT('',(-5.80203114222622,-1.95058727456727,2.44941649221591E-32));
#19846=CARTESIAN_POINT('Origin',(-5.19615242270666,-2.99999999999995,0.));
#19847=CARTESIAN_POINT('Origin',(-6.,6.24500451351651E-14,0.));
#19848=CARTESIAN_POINT('',(-6.00000000000001,-1.21175743903909,9.08672536706077E-33));
#19849=CARTESIAN_POINT('',(-5.99999999999999,1.21175743903921,9.08672536706164E-33));
#19850=CARTESIAN_POINT('Origin',(-6.,6.24500451351651E-14,0.));
#19851=CARTESIAN_POINT('Origin',(-5.1961524227066,3.00000000000006,0.));
#19852=CARTESIAN_POINT('',(-5.80203114222618,1.95058727456739,2.44941649221591E-32));
#19853=CARTESIAN_POINT('',(-4.59027370318701,4.04941272543273,-6.32071418803668E-33));
#19854=CARTESIAN_POINT('Origin',(-5.1961524227066,3.00000000000006,0.));
#19855=CARTESIAN_POINT('Origin',(-2.99999999999993,5.19615242270667,0.));
#19856=CARTESIAN_POINT('',(-4.04941272543262,4.59027370318711,1.38300558951226E-33));
#19857=CARTESIAN_POINT('',(-1.95058727456725,5.80203114222623,1.67904451446101E-32));
#19858=CARTESIAN_POINT('Origin',(-2.99999999999993,5.19615242270667,0.));
#19859=CARTESIAN_POINT('Origin',(0.,0.,2.5));
#19860=CARTESIAN_POINT('',(-6.48351648351648,-7.94001770875757E-16,2.375));
#19861=CARTESIAN_POINT('Origin',(0.,0.,2.375));
#19862=CARTESIAN_POINT('',(-6.48351648351648,-7.94001770875757E-16,1.21175743903915));
#19863=CARTESIAN_POINT('',(-6.48351648351648,-7.94001770875757E-16,2.5));
#19864=CARTESIAN_POINT('Origin',(0.,0.,1.21175743903915));
#19865=CARTESIAN_POINT('Origin',(0.,0.,2.5));
#19866=CARTESIAN_POINT('',(-5.51648351648352,-6.75574388101067E-16,1.21175743903915));
#19867=CARTESIAN_POINT('Origin',(0.,0.,1.21175743903915));
#19868=CARTESIAN_POINT('',(-5.51648351648352,-6.75574388101067E-16,2.375));
#19869=CARTESIAN_POINT('',(-5.51648351648352,-6.75574388101067E-16,2.5));
#19870=CARTESIAN_POINT('Origin',(0.,0.,2.375));
#19871=CARTESIAN_POINT('Origin',(0.,6.48351648351649,2.375));
#19872=CARTESIAN_POINT('Origin',(0.,6.48351648351649,1.21175743903915));
#19873=CARTESIAN_POINT('Origin',(0.,0.,2.5));
#19874=CARTESIAN_POINT('',(-6.48351648351649,-7.94001770875757E-16,-1.21175743903915));
#19875=CARTESIAN_POINT('Origin',(0.,0.,-1.21175743903915));
#19876=CARTESIAN_POINT('',(-6.48351648351649,-7.94001770875757E-16,-2.375));
#19877=CARTESIAN_POINT('',(-6.48351648351649,-7.94001770875757E-16,2.5));
#19878=CARTESIAN_POINT('Origin',(0.,0.,-2.375));
#19879=CARTESIAN_POINT('Origin',(0.,0.,2.5));
#19880=CARTESIAN_POINT('',(-5.51648351648352,-6.75574388101067E-16,-2.375));
#19881=CARTESIAN_POINT('Origin',(0.,0.,-2.375));
#19882=CARTESIAN_POINT('',(-5.51648351648352,-6.75574388101067E-16,-1.21175743903915));
#19883=CARTESIAN_POINT('',(-5.51648351648352,-6.75574388101067E-16,2.5));
#19884=CARTESIAN_POINT('Origin',(0.,0.,-1.21175743903915));
#19885=CARTESIAN_POINT('Origin',(0.,6.48351648351649,-2.375));
#19886=CARTESIAN_POINT('Origin',(0.,6.48351648351649,-1.21175743903915));
#19887=CARTESIAN_POINT('Origin',(0.,0.,-2.5));
#19888=CARTESIAN_POINT('',(9.,-1.10218211923262E-15,-2.5));
#19889=CARTESIAN_POINT('Origin',(0.,0.,-2.5));
#19890=CARTESIAN_POINT('',(9.,-1.10218211923262E-15,-1.4));
#19891=CARTESIAN_POINT('',(9.,-1.10218211923262E-15,-2.5));
#19892=CARTESIAN_POINT('Origin',(0.,0.,-1.4));
#19893=CARTESIAN_POINT('Origin',(0.,0.,2.5));
#19894=CARTESIAN_POINT('',(-6.48351648351648,-7.94001770875757E-16,1.11111111111111));
#19895=CARTESIAN_POINT('Origin',(0.,0.,1.11111111111111));
#19896=CARTESIAN_POINT('',(-6.48351648351648,-7.94001770875757E-16,2.5));
#19897=CARTESIAN_POINT('',(-6.48351648351648,-7.94001770875757E-16,2.5));
#19898=CARTESIAN_POINT('Origin',(0.,0.,2.5));
#19899=CARTESIAN_POINT('Origin',(0.,0.,0.));
#19900=CARTESIAN_POINT('',(-6.48351648351648,-7.94001770875757E-16,-1.11111111111111));
#19901=CARTESIAN_POINT('Origin',(0.,0.,-1.11111111111111));
#19902=CARTESIAN_POINT('Origin',(-6.,-7.34788079488412E-16,0.));
#19903=CARTESIAN_POINT('Origin',(0.,0.,2.5));
#19904=CARTESIAN_POINT('',(-6.48351648351648,-7.94001770875757E-16,-2.5));
#19905=CARTESIAN_POINT('Origin',(0.,0.,-2.5));
#19906=CARTESIAN_POINT('',(-6.48351648351648,-7.94001770875757E-16,2.5));
#19907=CARTESIAN_POINT('Origin',(0.,0.,2.5));
#19908=CARTESIAN_POINT('',(8.,9.79717439317883E-16,2.25));
#19909=CARTESIAN_POINT('',(-8.,-9.79717439317883E-16,2.25));
#19910=CARTESIAN_POINT('Origin',(0.,0.,2.25));
#19911=CARTESIAN_POINT('Origin',(0.,0.,2.25));
#19912=CARTESIAN_POINT('',(-8.,-9.79717439317883E-16,-1.4));
#19913=CARTESIAN_POINT('',(-8.,-9.79717439317883E-16,2.5));
#19914=CARTESIAN_POINT('Origin',(0.,0.,-1.4));
#19915=CARTESIAN_POINT('Origin',(0.,0.,2.25));
#19916=CARTESIAN_POINT('',(7.75,-9.49101269339199E-16,2.5));
#19917=CARTESIAN_POINT('',(8.,-9.79717439317883E-16,2.25));
#19918=CARTESIAN_POINT('Origin',(0.,0.,2.5));
#19919=CARTESIAN_POINT('Origin',(0.,7.75,-2.5));
#19920=CARTESIAN_POINT('Origin',(0.,7.75,2.5));
#19921=CARTESIAN_POINT('Origin',(0.,6.48351648351649,-1.4));
#19922=CARTESIAN_POINT('',(0.,0.,0.));
#19923=CARTESIAN_POINT('Origin',(0.,0.,12.4));
#19924=CARTESIAN_POINT('',(5.,-6.12323399573677E-16,0.));
#19925=CARTESIAN_POINT('Origin',(0.,0.,0.));
#19926=CARTESIAN_POINT('',(5.,-6.12323399573677E-16,12.4));
#19927=CARTESIAN_POINT('',(5.,-6.12323399573677E-16,12.4));
#19928=CARTESIAN_POINT('Origin',(0.,0.,12.4));
#19929=CARTESIAN_POINT('Origin',(0.,0.,23.));
#19930=CARTESIAN_POINT('',(2.1,-2.57175827820944E-16,23.));
#19931=CARTESIAN_POINT('Origin',(0.,0.,23.));
#19932=CARTESIAN_POINT('',(2.1,-2.57175827820944E-16,0.));
#19933=CARTESIAN_POINT('',(2.1,-2.57175827820944E-16,23.));
#19934=CARTESIAN_POINT('Origin',(0.,0.,0.));
#19935=CARTESIAN_POINT('Origin',(0.,0.,23.));
#19936=CARTESIAN_POINT('',(4.,-4.89858719658941E-16,12.4));
#19937=CARTESIAN_POINT('Origin',(0.,0.,12.4));
#19938=CARTESIAN_POINT('',(4.,-4.89858719658941E-16,23.));
#19939=CARTESIAN_POINT('',(4.,-4.89858719658941E-16,23.));
#19940=CARTESIAN_POINT('Origin',(0.,0.,23.));
#19941=CARTESIAN_POINT('Origin',(0.,0.,23.));
#19942=CARTESIAN_POINT('Origin',(0.,0.,0.));
#19943=CARTESIAN_POINT('Origin',(0.,0.,12.4));
#19944=CARTESIAN_POINT('',(0.,0.,0.));
#19945=CARTESIAN_POINT('Origin',(-4.33680868994202E-15,-2.08166817117217E-14,
12.4));
#19946=CARTESIAN_POINT('',(4.99999999999999,-1.80983360374199E-14,0.));
#19947=CARTESIAN_POINT('Origin',(0.,0.,0.));
#19948=CARTESIAN_POINT('',(4.99999999999999,-1.80983360374199E-14,12.4));
#19949=CARTESIAN_POINT('',(4.99999999999999,-1.80983360374199E-14,12.4));
#19950=CARTESIAN_POINT('Origin',(-4.33680868994202E-15,-2.08166817117217E-14,
12.4));
#19951=CARTESIAN_POINT('Origin',(-3.46944695195361E-15,-2.08166817117217E-14,
23.));
#19952=CARTESIAN_POINT('',(1.6,-1.99468110959451E-14,23.));
#19953=CARTESIAN_POINT('Origin',(-3.46944695195361E-15,-2.08166817117217E-14,
23.));
#19954=CARTESIAN_POINT('',(1.6,-1.99468110959451E-14,0.));
#19955=CARTESIAN_POINT('',(1.6,-1.99468110959451E-14,23.));
#19956=CARTESIAN_POINT('Origin',(0.,0.,0.));
#19957=CARTESIAN_POINT('Origin',(-3.46944695195361E-15,-2.08166817117217E-14,
23.));
#19958=CARTESIAN_POINT('',(4.,-1.86420051722803E-14,12.4));
#19959=CARTESIAN_POINT('Origin',(-4.33680868994202E-15,-2.08166817117217E-14,
12.4));
#19960=CARTESIAN_POINT('',(4.,-1.86420051722803E-14,23.));
#19961=CARTESIAN_POINT('',(4.,-1.86420051722803E-14,23.));
#19962=CARTESIAN_POINT('Origin',(-3.46944695195361E-15,-2.08166817117217E-14,
23.));
#19963=CARTESIAN_POINT('Origin',(-3.46944695195361E-15,-2.08166817117217E-14,
23.));
#19964=CARTESIAN_POINT('Origin',(0.,0.,0.));
#19965=CARTESIAN_POINT('Origin',(-4.33680868994202E-15,-2.08166817117217E-14,
12.4));
#19966=CARTESIAN_POINT('',(-13.6605841442288,-43.1227702405477,36.5054777336268));
#19967=CARTESIAN_POINT('',(-39.6605841442288,-14.5227702405477,24.5054777336268));
#19968=CARTESIAN_POINT('',(-19.6605841442288,-23.1227702405477,-47.4945222663731));
#19969=CARTESIAN_POINT('',(-39.6605841442288,0.377229759452348,24.5054777336268));
#19970=CARTESIAN_POINT('',(-39.6605841442288,-46.6227702405476,24.5054777336268));
#19971=CARTESIAN_POINT('',(-39.6605841442288,-31.7227702405476,24.5054777336268));
#19972=CARTESIAN_POINT('',(-1.66058414422877,-31.7227702405476,36.5054777336268));
#19973=CARTESIAN_POINT('',(-1.66058414422877,-14.5227702405477,36.5054777336268));
#19974=CARTESIAN_POINT('',(-1.66058414422877,0.377229759452344,36.5054777336268));
#19975=CARTESIAN_POINT('',(-1.66058414422877,-46.6227702405476,36.5054777336268));
#19976=CARTESIAN_POINT('',(-7.84159634540629,7.2563035870985,-0.791922048193099));
#19977=CARTESIAN_POINT('',(5.15840365459371,15.8563035870985,18.7080779518069));
#19978=CARTESIAN_POINT('',(5.15840365459371,-1.3436964129015,18.7080779518069));
#19979=CARTESIAN_POINT('',(5.15840365459371,30.7563035870985,18.7080779518069));
#19980=CARTESIAN_POINT('',(5.15840365459371,-16.2436964129015,18.7080779518069));
#19981=CARTESIAN_POINT('',(0.,0.,0.));
#19982=CARTESIAN_POINT('Origin',(0.,5.,-40.));
#19983=CARTESIAN_POINT('',(-2.75545529808153E-16,2.66,-42.25));
#19984=CARTESIAN_POINT('Origin',(0.,2.66000000000001,-40.));
#19985=CARTESIAN_POINT('',(-5.62112880808636E-16,5.,-44.59));
#19986=CARTESIAN_POINT('',(-5.62112880808636E-16,5.,-44.59));
#19987=CARTESIAN_POINT('Origin',(0.,5.,-40.));
#19988=CARTESIAN_POINT('Origin',(0.,5.,-40.));
#19989=CARTESIAN_POINT('',(-2.75545529808153E-16,-4.44089209850063E-15,
-42.25));
#19990=CARTESIAN_POINT('Origin',(0.,-4.33680868994202E-15,-40.));
#19991=CARTESIAN_POINT('',(-2.75545529808153E-16,5.,-42.25));
#19992=CARTESIAN_POINT('Origin',(0.,5.,0.));
#19993=CARTESIAN_POINT('',(-2.75545529808153E-16,2.66000000000001,-2.24999999999999));
#19994=CARTESIAN_POINT('Origin',(0.,2.66000000000001,0.));
#19995=CARTESIAN_POINT('',(-5.62112880808635E-16,5.,-4.59));
#19996=CARTESIAN_POINT('',(-5.62112880808635E-16,5.,-4.59));
#19997=CARTESIAN_POINT('Origin',(0.,5.,0.));
#19998=CARTESIAN_POINT('Origin',(0.,5.,0.));
#19999=CARTESIAN_POINT('',(-2.75545529808153E-16,-4.44089209850063E-15,
-2.24999999999999));
#20000=CARTESIAN_POINT('Origin',(0.,-4.33680868994202E-15,0.));
#20001=CARTESIAN_POINT('',(-2.75545529808153E-16,5.,-2.24999999999999));
#20002=CARTESIAN_POINT('Origin',(0.,5.,-40.));
#20003=CARTESIAN_POINT('',(10.,5.,-40.));
#20004=CARTESIAN_POINT('',(-10.,5.,-40.));
#20005=CARTESIAN_POINT('Origin',(0.,5.,-40.));
#20006=CARTESIAN_POINT('',(10.,0.,-40.));
#20007=CARTESIAN_POINT('',(10.,5.,-40.));
#20008=CARTESIAN_POINT('',(-10.,0.,-40.));
#20009=CARTESIAN_POINT('Origin',(0.,0.,-40.));
#20010=CARTESIAN_POINT('',(-10.,5.,-40.));
#20011=CARTESIAN_POINT('Origin',(0.,5.,0.));
#20012=CARTESIAN_POINT('',(-10.,5.,0.));
#20013=CARTESIAN_POINT('',(10.,5.,0.));
#20014=CARTESIAN_POINT('Origin',(0.,5.,0.));
#20015=CARTESIAN_POINT('',(10.,5.,0.));
#20016=CARTESIAN_POINT('',(-10.,5.,0.));
#20017=CARTESIAN_POINT('Origin',(0.,0.,0.));
#20018=CARTESIAN_POINT('',(-10.,0.,0.));
#20019=CARTESIAN_POINT('',(10.,0.,0.));
#20020=CARTESIAN_POINT('Origin',(0.,0.,0.));
#20021=CARTESIAN_POINT('',(-10.,0.,0.));
#20022=CARTESIAN_POINT('',(10.,0.,0.));
#20023=CARTESIAN_POINT('Origin',(0.,5.,0.));
#20024=CARTESIAN_POINT('',(10.,5.,0.));
#20025=CARTESIAN_POINT('',(-10.,5.,0.));
#20026=CARTESIAN_POINT('Origin',(10.,5.,0.));
#20027=CARTESIAN_POINT('Origin',(-10.,5.,0.));
#20028=CARTESIAN_POINT('',(0.,0.,0.));
#20029=CARTESIAN_POINT('Origin',(1.5,0.,0.));
#20030=CARTESIAN_POINT('',(2.22168783648704,-1.82728999845763E-16,0.));
#20031=CARTESIAN_POINT('',(1.5,7.5115729936858E-16,-1.25));
#20032=CARTESIAN_POINT('',(1.5,-1.53080849893419E-16,-1.25));
#20033=CARTESIAN_POINT('',(1.5,-1.08253175473055,-0.625000000000001));
#20034=CARTESIAN_POINT('Origin',(1.5,0.,0.));
#20035=CARTESIAN_POINT('',(1.5,-1.08253175473055,0.625000000000002));
#20036=CARTESIAN_POINT('Origin',(1.5,0.,0.));
#20037=CARTESIAN_POINT('',(1.5,0.,1.25));
#20038=CARTESIAN_POINT('Origin',(1.5,0.,0.));
#20039=CARTESIAN_POINT('',(1.5,1.08253175473055,0.625));
#20040=CARTESIAN_POINT('Origin',(1.5,0.,0.));
#20041=CARTESIAN_POINT('',(1.5,1.08253175473055,-0.625000000000001));
#20042=CARTESIAN_POINT('Origin',(1.5,0.,0.));
#20043=CARTESIAN_POINT('Origin',(1.5,0.,0.));
#20044=CARTESIAN_POINT('Origin',(2.56284271247462,0.,0.));
#20045=CARTESIAN_POINT('',(2.42142135623731,-2.52103174687708E-16,-2.05857864376269));
#20046=CARTESIAN_POINT('Origin',(2.42142135623731,0.,0.));
#20047=CARTESIAN_POINT('',(2.56284271247462,-2.4492935982947E-16,-2.));
#20048=CARTESIAN_POINT('Origin',(2.56284271247462,-2.69422295812418E-16,
-2.2));
#20049=CARTESIAN_POINT('Origin',(2.56284271247462,0.,0.));
#20050=CARTESIAN_POINT('Origin',(0.,0.,0.));
#20051=CARTESIAN_POINT('',(0.,-4.77612251667468E-16,-3.9));
#20052=CARTESIAN_POINT('Origin',(0.,0.,0.));
#20053=CARTESIAN_POINT('',(0.580000000000009,-4.77612251667468E-16,-3.9));
#20054=CARTESIAN_POINT('',(0.,-4.77612251667468E-16,-3.9));
#20055=CARTESIAN_POINT('Origin',(0.580000000000009,0.,0.));
#20056=CARTESIAN_POINT('Origin',(0.580000000000009,0.,0.));
#20057=CARTESIAN_POINT('',(0.580000000000009,-4.77612251667468E-16,-3.9));
#20058=CARTESIAN_POINT('Origin',(0.,0.,0.));
#20059=CARTESIAN_POINT('',(15.61,-2.4492935982947E-16,-2.));
#20060=CARTESIAN_POINT('',(0.,-2.4492935982947E-16,-2.));
#20061=CARTESIAN_POINT('Origin',(15.61,0.,0.));
#20062=CARTESIAN_POINT('Origin',(16.,0.,0.));
#20063=CARTESIAN_POINT('',(16.,-1.97168134662724E-16,-1.61));
#20064=CARTESIAN_POINT('',(16.,-1.97168134662724E-16,-1.61));
#20065=CARTESIAN_POINT('Origin',(16.,0.,0.));
#20066=CARTESIAN_POINT('Origin',(0.,0.,0.));
#20067=CARTESIAN_POINT('',(0.,-0.721687836487031,1.25));
#20068=CARTESIAN_POINT('',(0.,-1.44337567297407,3.25260651745651E-16));
#20069=CARTESIAN_POINT('',(0.,-0.721687836487031,1.25));
#20070=CARTESIAN_POINT('',(0.,-0.721687836487032,-1.25));
#20071=CARTESIAN_POINT('',(0.,-1.44337567297407,3.72758124193626E-16));
#20072=CARTESIAN_POINT('',(0.,0.721687836487033,-1.25));
#20073=CARTESIAN_POINT('',(0.,-0.721687836487032,-1.25));
#20074=CARTESIAN_POINT('',(0.,1.44337567297407,-3.23360327335785E-17));
#20075=CARTESIAN_POINT('',(0.,0.721687836487033,-1.25));
#20076=CARTESIAN_POINT('',(0.,0.721687836487033,1.25));
#20077=CARTESIAN_POINT('',(0.,1.44337567297407,-3.23360327335785E-17));
#20078=CARTESIAN_POINT('',(0.,0.721687836487033,1.25));
#20079=CARTESIAN_POINT('Origin',(16.,1.61,0.));
#20080=CARTESIAN_POINT('Origin',(1.5,-1.44337567297407,3.72758124193626E-16));
#20081=CARTESIAN_POINT('',(1.5,-1.44337567297407,3.72758124193626E-16));
#20082=CARTESIAN_POINT('',(1.5,-1.44337567297407,3.72758124193626E-16));
#20083=CARTESIAN_POINT('',(1.5,-1.44337567297407,3.72758124193626E-16));
#20084=CARTESIAN_POINT('',(1.5,-0.721687836487032,-1.25));
#20085=CARTESIAN_POINT('',(1.5,-1.44337567297407,3.72758124193626E-16));
#20086=CARTESIAN_POINT('',(1.5,-0.721687836487032,-1.25));
#20087=CARTESIAN_POINT('Origin',(1.5,-0.721687836487032,-1.25));
#20088=CARTESIAN_POINT('',(1.5,-0.721687836487032,-1.25));
#20089=CARTESIAN_POINT('',(1.5,0.721687836487033,-1.25));
#20090=CARTESIAN_POINT('',(1.5,-0.721687836487032,-1.25));
#20091=CARTESIAN_POINT('',(1.5,0.721687836487033,-1.25));
#20092=CARTESIAN_POINT('Origin',(1.5,0.721687836487033,-1.25));
#20093=CARTESIAN_POINT('',(1.5,0.721687836487033,-1.25));
#20094=CARTESIAN_POINT('',(1.5,1.44337567297407,-3.23360327335785E-17));
#20095=CARTESIAN_POINT('',(1.5,0.721687836487033,-1.25));
#20096=CARTESIAN_POINT('',(1.5,1.44337567297407,-3.23360327335785E-17));
#20097=CARTESIAN_POINT('Origin',(1.5,1.44337567297407,-3.23360327335785E-17));
#20098=CARTESIAN_POINT('',(1.5,1.44337567297407,-3.23360327335785E-17));
#20099=CARTESIAN_POINT('',(1.5,0.721687836487033,1.25));
#20100=CARTESIAN_POINT('',(1.5,1.44337567297407,-3.23360327335785E-17));
#20101=CARTESIAN_POINT('',(1.5,0.721687836487033,1.25));
#20102=CARTESIAN_POINT('Origin',(1.5,0.721687836487033,1.25));
#20103=CARTESIAN_POINT('',(1.5,0.721687836487033,1.25));
#20104=CARTESIAN_POINT('',(1.5,-0.721687836487031,1.25));
#20105=CARTESIAN_POINT('',(1.5,0.721687836487033,1.25));
#20106=CARTESIAN_POINT('',(1.5,-0.721687836487031,1.25));
#20107=CARTESIAN_POINT('Origin',(1.5,-0.721687836487031,1.25));
#20108=CARTESIAN_POINT('',(1.5,-0.721687836487031,1.25));
#20109=CARTESIAN_POINT('',(1.5,-0.721687836487031,1.25));
#20110=CARTESIAN_POINT('Origin',(1.5,-1.44337567297407,4.33680868994202E-16));
#20111=CARTESIAN_POINT('Origin',(1.5,-1.44337567297407,4.33680868994202E-16));
#20112=CARTESIAN_POINT('Origin',(1.5,-1.44337567297407,4.33680868994202E-16));
#20113=CARTESIAN_POINT('Origin',(1.5,-1.44337567297407,4.33680868994202E-16));
#20114=CARTESIAN_POINT('Origin',(1.5,-1.44337567297407,4.33680868994202E-16));
#20115=CARTESIAN_POINT('Origin',(1.5,-1.44337567297407,4.33680868994202E-16));
#20116=CARTESIAN_POINT('',(0.,0.,0.));
#20117=CARTESIAN_POINT('',(-6.99999999999999,1.15554797274006E-15,-24.));
#20118=CARTESIAN_POINT('',(-52.5000000000001,-1.04083408558608E-14,-68.1));
#20119=CARTESIAN_POINT('',(3.41817158503853E-21,23.5,-3.26136119688951E-16));
#20120=CARTESIAN_POINT('',(22.3794572057247,28.39,33.1535804277176));
#20121=CARTESIAN_POINT('',(-11.9999999999999,-23.5,38.));
#20122=CARTESIAN_POINT('',(46.8849349393506,23.1227702405476,72.8141645719467));
#20123=CARTESIAN_POINT('',(6.7080779518069,-7.2563035870985,32.8415963454063));
#20124=CARTESIAN_POINT('',(-7.45464222593552E-16,1.1970459345978E-14,-48.));
#20125=CARTESIAN_POINT('',(-7.,1.03820556882806E-17,-24.));
#20126=CARTESIAN_POINT('',(1.4335689156505E-22,-23.5,3.26133034793875E-16));
#20127=CARTESIAN_POINT('',(22.3794572057247,-28.39,33.1535804277176));
#20128=CARTESIAN_POINT('',(10.3794572057247,28.39,71.1535804277176));
#20129=CARTESIAN_POINT('',(-12.,28.39,38.));
#20130=CARTESIAN_POINT('',(10.3794572057247,-28.39,71.1535804277176));
#20131=CARTESIAN_POINT('',(-12.,-28.39,38.));
#20132=CARTESIAN_POINT('',(-11.9999999999998,23.5,38.0000000000001));
#20133=CARTESIAN_POINT('',(-3.53360651949483E-15,-23.5,-48.));
#20134=CARTESIAN_POINT('',(6.8387467485498E-15,23.5,-48.));
#20135=CARTESIAN_POINT('',(39.957797077546,-23.1227702405476,-124.555378179344));
#20136=CARTESIAN_POINT('',(6.7080779518069,7.25630358709851,-80.8415963454062));
#20137=CARTESIAN_POINT('',(-12.,23.5,-86.));
#20138=CARTESIAN_POINT('',(-12.,-23.5,-86.));
#20139=CARTESIAN_POINT('',(15.4523193439192,-28.39,-84.8947940351148));
#20140=CARTESIAN_POINT('',(3.45231934391922,-28.39,-122.894794035115));
#20141=CARTESIAN_POINT('',(-12.,-28.39,-86.));
#20142=CARTESIAN_POINT('',(3.45231934391921,28.39,-122.894794035115));
#20143=CARTESIAN_POINT('',(-12.,28.39,-86.));
#20144=CARTESIAN_POINT('',(15.4523193439192,28.39,-84.8947940351148));
#20145=UNCERTAINTY_MEASURE_WITH_UNIT(LENGTH_MEASURE(0.01),#20177,
'DISTANCE_ACCURACY_VALUE',
'Maximum model space distance between geometric entities at asserted c
onnectivities');
#20146=UNCERTAINTY_MEASURE_WITH_UNIT(LENGTH_MEASURE(0.01),#20177,
'DISTANCE_ACCURACY_VALUE',
'Maximum model space distance between geometric entities at asserted c
onnectivities');
#20147=UNCERTAINTY_MEASURE_WITH_UNIT(LENGTH_MEASURE(0.01),#20177,
'DISTANCE_ACCURACY_VALUE',
'Maximum model space distance between geometric entities at asserted c
onnectivities');
#20148=UNCERTAINTY_MEASURE_WITH_UNIT(LENGTH_MEASURE(0.01),#20177,
'DISTANCE_ACCURACY_VALUE',
'Maximum model space distance between geometric entities at asserted c
onnectivities');
#20149=UNCERTAINTY_MEASURE_WITH_UNIT(LENGTH_MEASURE(0.01),#20177,
'DISTANCE_ACCURACY_VALUE',
'Maximum model space distance between geometric entities at asserted c
onnectivities');
#20150=UNCERTAINTY_MEASURE_WITH_UNIT(LENGTH_MEASURE(0.01),#20177,
'DISTANCE_ACCURACY_VALUE',
'Maximum model space distance between geometric entities at asserted c
onnectivities');
#20151=UNCERTAINTY_MEASURE_WITH_UNIT(LENGTH_MEASURE(0.01),#20177,
'DISTANCE_ACCURACY_VALUE',
'Maximum model space distance between geometric entities at asserted c
onnectivities');
#20152=UNCERTAINTY_MEASURE_WITH_UNIT(LENGTH_MEASURE(0.01),#20177,
'DISTANCE_ACCURACY_VALUE',
'Maximum model space distance between geometric entities at asserted c
onnectivities');
#20153=UNCERTAINTY_MEASURE_WITH_UNIT(LENGTH_MEASURE(0.01),#20177,
'DISTANCE_ACCURACY_VALUE',
'Maximum model space distance between geometric entities at asserted c
onnectivities');
#20154=UNCERTAINTY_MEASURE_WITH_UNIT(LENGTH_MEASURE(0.01),#20177,
'DISTANCE_ACCURACY_VALUE',
'Maximum model space distance between geometric entities at asserted c
onnectivities');
#20155=UNCERTAINTY_MEASURE_WITH_UNIT(LENGTH_MEASURE(0.01),#20177,
'DISTANCE_ACCURACY_VALUE',
'Maximum model space distance between geometric entities at asserted c
onnectivities');
#20156=UNCERTAINTY_MEASURE_WITH_UNIT(LENGTH_MEASURE(0.01),#20177,
'DISTANCE_ACCURACY_VALUE',
'Maximum model space distance between geometric entities at asserted c
onnectivities');
#20157=UNCERTAINTY_MEASURE_WITH_UNIT(LENGTH_MEASURE(0.01),#20177,
'DISTANCE_ACCURACY_VALUE',
'Maximum model space distance between geometric entities at asserted c
onnectivities');
#20158=UNCERTAINTY_MEASURE_WITH_UNIT(LENGTH_MEASURE(0.01),#20177,
'DISTANCE_ACCURACY_VALUE',
'Maximum model space distance between geometric entities at asserted c
onnectivities');
#20159=UNCERTAINTY_MEASURE_WITH_UNIT(LENGTH_MEASURE(0.01),#20177,
'DISTANCE_ACCURACY_VALUE',
'Maximum model space distance between geometric entities at asserted c
onnectivities');
#20160=UNCERTAINTY_MEASURE_WITH_UNIT(LENGTH_MEASURE(0.01),#20177,
'DISTANCE_ACCURACY_VALUE',
'Maximum model space distance between geometric entities at asserted c
onnectivities');
#20161=(
GEOMETRIC_REPRESENTATION_CONTEXT(3)
GLOBAL_UNCERTAINTY_ASSIGNED_CONTEXT((#20145))
GLOBAL_UNIT_ASSIGNED_CONTEXT((#20177,#20179,#20180))
REPRESENTATION_CONTEXT('','3D')
);
#20162=(
GEOMETRIC_REPRESENTATION_CONTEXT(3)
GLOBAL_UNCERTAINTY_ASSIGNED_CONTEXT((#20146))
GLOBAL_UNIT_ASSIGNED_CONTEXT((#20177,#20179,#20180))
REPRESENTATION_CONTEXT('','3D')
);
#20163=(
GEOMETRIC_REPRESENTATION_CONTEXT(3)
GLOBAL_UNCERTAINTY_ASSIGNED_CONTEXT((#20147))
GLOBAL_UNIT_ASSIGNED_CONTEXT((#20177,#20179,#20180))
REPRESENTATION_CONTEXT('','3D')
);
#20164=(
GEOMETRIC_REPRESENTATION_CONTEXT(3)
GLOBAL_UNCERTAINTY_ASSIGNED_CONTEXT((#20148))
GLOBAL_UNIT_ASSIGNED_CONTEXT((#20177,#20179,#20180))
REPRESENTATION_CONTEXT('','3D')
);
#20165=(
GEOMETRIC_REPRESENTATION_CONTEXT(3)
GLOBAL_UNCERTAINTY_ASSIGNED_CONTEXT((#20149))
GLOBAL_UNIT_ASSIGNED_CONTEXT((#20177,#20179,#20180))
REPRESENTATION_CONTEXT('','3D')
);
#20166=(
GEOMETRIC_REPRESENTATION_CONTEXT(3)
GLOBAL_UNCERTAINTY_ASSIGNED_CONTEXT((#20150))
GLOBAL_UNIT_ASSIGNED_CONTEXT((#20177,#20179,#20180))
REPRESENTATION_CONTEXT('','3D')
);
#20167=(
GEOMETRIC_REPRESENTATION_CONTEXT(3)
GLOBAL_UNCERTAINTY_ASSIGNED_CONTEXT((#20151))
GLOBAL_UNIT_ASSIGNED_CONTEXT((#20177,#20179,#20180))
REPRESENTATION_CONTEXT('','3D')
);
#20168=(
GEOMETRIC_REPRESENTATION_CONTEXT(3)
GLOBAL_UNCERTAINTY_ASSIGNED_CONTEXT((#20152))
GLOBAL_UNIT_ASSIGNED_CONTEXT((#20177,#20179,#20180))
REPRESENTATION_CONTEXT('','3D')
);
#20169=(
GEOMETRIC_REPRESENTATION_CONTEXT(3)
GLOBAL_UNCERTAINTY_ASSIGNED_CONTEXT((#20153))
GLOBAL_UNIT_ASSIGNED_CONTEXT((#20177,#20179,#20180))
REPRESENTATION_CONTEXT('','3D')
);
#20170=(
GEOMETRIC_REPRESENTATION_CONTEXT(3)
GLOBAL_UNCERTAINTY_ASSIGNED_CONTEXT((#20154))
GLOBAL_UNIT_ASSIGNED_CONTEXT((#20177,#20179,#20180))
REPRESENTATION_CONTEXT('','3D')
);
#20171=(
GEOMETRIC_REPRESENTATION_CONTEXT(3)
GLOBAL_UNCERTAINTY_ASSIGNED_CONTEXT((#20155))
GLOBAL_UNIT_ASSIGNED_CONTEXT((#20177,#20179,#20180))
REPRESENTATION_CONTEXT('','3D')
);
#20172=(
GEOMETRIC_REPRESENTATION_CONTEXT(3)
GLOBAL_UNCERTAINTY_ASSIGNED_CONTEXT((#20156))
GLOBAL_UNIT_ASSIGNED_CONTEXT((#20177,#20179,#20180))
REPRESENTATION_CONTEXT('','3D')
);
#20173=(
GEOMETRIC_REPRESENTATION_CONTEXT(3)
GLOBAL_UNCERTAINTY_ASSIGNED_CONTEXT((#20157))
GLOBAL_UNIT_ASSIGNED_CONTEXT((#20177,#20179,#20180))
REPRESENTATION_CONTEXT('','3D')
);
#20174=(
GEOMETRIC_REPRESENTATION_CONTEXT(3)
GLOBAL_UNCERTAINTY_ASSIGNED_CONTEXT((#20158))
GLOBAL_UNIT_ASSIGNED_CONTEXT((#20177,#20179,#20180))
REPRESENTATION_CONTEXT('','3D')
);
#20175=(
GEOMETRIC_REPRESENTATION_CONTEXT(3)
GLOBAL_UNCERTAINTY_ASSIGNED_CONTEXT((#20159))
GLOBAL_UNIT_ASSIGNED_CONTEXT((#20177,#20179,#20180))
REPRESENTATION_CONTEXT('','3D')
);
#20176=(
GEOMETRIC_REPRESENTATION_CONTEXT(3)
GLOBAL_UNCERTAINTY_ASSIGNED_CONTEXT((#20160))
GLOBAL_UNIT_ASSIGNED_CONTEXT((#20177,#20179,#20180))
REPRESENTATION_CONTEXT('','3D')
);
#20177=(
LENGTH_UNIT()
NAMED_UNIT(*)
SI_UNIT(.MILLI.,.METRE.)
);
#20178=(
LENGTH_UNIT()
NAMED_UNIT(*)
SI_UNIT($,.METRE.)
);
#20179=(
NAMED_UNIT(*)
PLANE_ANGLE_UNIT()
SI_UNIT($,.RADIAN.)
);
#20180=(
NAMED_UNIT(*)
SI_UNIT($,.STERADIAN.)
SOLID_ANGLE_UNIT()
);
#20181=SHAPE_DEFINITION_REPRESENTATION(#20196,#20255);
#20182=SHAPE_DEFINITION_REPRESENTATION(#20197,#20256);
#20183=SHAPE_DEFINITION_REPRESENTATION(#20198,#20257);
#20184=SHAPE_DEFINITION_REPRESENTATION(#20199,#20258);
#20185=SHAPE_DEFINITION_REPRESENTATION(#20200,#20259);
#20186=SHAPE_DEFINITION_REPRESENTATION(#20201,#20260);
#20187=SHAPE_DEFINITION_REPRESENTATION(#20202,#20261);
#20188=SHAPE_DEFINITION_REPRESENTATION(#20203,#20262);
#20189=SHAPE_DEFINITION_REPRESENTATION(#20204,#20263);
#20190=SHAPE_DEFINITION_REPRESENTATION(#20205,#20264);
#20191=SHAPE_DEFINITION_REPRESENTATION(#20206,#20265);
#20192=SHAPE_DEFINITION_REPRESENTATION(#20207,#20266);
#20193=SHAPE_DEFINITION_REPRESENTATION(#20208,#20267);
#20194=SHAPE_DEFINITION_REPRESENTATION(#20224,#20268);
#20195=SHAPE_DEFINITION_REPRESENTATION(#20225,#20269);
#20196=PRODUCT_DEFINITION_SHAPE('',$,#20271);
#20197=PRODUCT_DEFINITION_SHAPE('',$,#20272);
#20198=PRODUCT_DEFINITION_SHAPE('',$,#20273);
#20199=PRODUCT_DEFINITION_SHAPE('',$,#20274);
#20200=PRODUCT_DEFINITION_SHAPE('',$,#20275);
#20201=PRODUCT_DEFINITION_SHAPE('',$,#20276);
#20202=PRODUCT_DEFINITION_SHAPE('',$,#20277);
#20203=PRODUCT_DEFINITION_SHAPE('',$,#20278);
#20204=PRODUCT_DEFINITION_SHAPE('',$,#20279);
#20205=PRODUCT_DEFINITION_SHAPE('',$,#20280);
#20206=PRODUCT_DEFINITION_SHAPE('',$,#20281);
#20207=PRODUCT_DEFINITION_SHAPE('',$,#20282);
#20208=PRODUCT_DEFINITION_SHAPE('',$,#20283);
#20209=PRODUCT_DEFINITION_SHAPE($,$,#143);
#20210=PRODUCT_DEFINITION_SHAPE($,$,#144);
#20211=PRODUCT_DEFINITION_SHAPE($,$,#145);
#20212=PRODUCT_DEFINITION_SHAPE($,$,#146);
#20213=PRODUCT_DEFINITION_SHAPE($,$,#147);
#20214=PRODUCT_DEFINITION_SHAPE($,$,#148);
#20215=PRODUCT_DEFINITION_SHAPE($,$,#149);
#20216=PRODUCT_DEFINITION_SHAPE($,$,#150);
#20217=PRODUCT_DEFINITION_SHAPE($,$,#151);
#20218=PRODUCT_DEFINITION_SHAPE($,$,#152);
#20219=PRODUCT_DEFINITION_SHAPE($,$,#153);
#20220=PRODUCT_DEFINITION_SHAPE($,$,#154);
#20221=PRODUCT_DEFINITION_SHAPE($,$,#155);
#20222=PRODUCT_DEFINITION_SHAPE($,$,#156);
#20223=PRODUCT_DEFINITION_SHAPE($,$,#157);
#20224=PRODUCT_DEFINITION_SHAPE('',$,#20284);
#20225=PRODUCT_DEFINITION_SHAPE('',$,#20285);
#20226=PRODUCT_DEFINITION_SHAPE($,$,#158);
#20227=PRODUCT_DEFINITION_SHAPE($,$,#159);
#20228=PRODUCT_DEFINITION_SHAPE($,$,#160);
#20229=PRODUCT_DEFINITION_SHAPE($,$,#161);
#20230=PRODUCT_DEFINITION_SHAPE($,$,#162);
#20231=PRODUCT_DEFINITION_SHAPE($,$,#163);
#20232=PRODUCT_DEFINITION_SHAPE($,$,#164);
#20233=PRODUCT_DEFINITION_SHAPE($,$,#165);
#20234=PRODUCT_DEFINITION_SHAPE($,$,#166);
#20235=PRODUCT_DEFINITION_SHAPE($,$,#167);
#20236=PRODUCT_DEFINITION_SHAPE($,$,#168);
#20237=PRODUCT_DEFINITION_SHAPE($,$,#169);
#20238=PRODUCT_DEFINITION_SHAPE($,$,#170);
#20239=PRODUCT_DEFINITION_SHAPE($,$,#171);
#20240=PRODUCT_DEFINITION_SHAPE($,$,#172);
#20241=PRODUCT_DEFINITION_SHAPE($,$,#173);
#20242=PRODUCT_DEFINITION_SHAPE($,$,#174);
#20243=PRODUCT_DEFINITION_SHAPE($,$,#175);
#20244=PRODUCT_DEFINITION_SHAPE($,$,#176);
#20245=PRODUCT_DEFINITION_SHAPE($,$,#177);
#20246=PRODUCT_DEFINITION_SHAPE($,$,#178);
#20247=PRODUCT_DEFINITION_SHAPE($,$,#179);
#20248=PRODUCT_DEFINITION_SHAPE($,$,#180);
#20249=PRODUCT_DEFINITION_SHAPE($,$,#181);
#20250=PRODUCT_DEFINITION_SHAPE($,$,#182);
#20251=PRODUCT_DEFINITION_SHAPE($,$,#183);
#20252=PRODUCT_DEFINITION_SHAPE($,$,#184);
#20253=PRODUCT_DEFINITION_SHAPE($,$,#185);
#20254=PRODUCT_DEFINITION_SHAPE($,$,#186);
#20255=SHAPE_REPRESENTATION('',(#11104,#12185,#12186,#12187,#12188,#12189,
#12190,#12191,#12192,#12193,#12194,#12195,#12196,#12197,#12198,#12199,#12200,
#12201,#12202,#12203,#12204,#12205,#12206,#12207,#12208,#12209,#12210,#12211,
#12212,#12213),#20161);
#20256=SHAPE_REPRESENTATION('',(#11105),#20162);
#20257=SHAPE_REPRESENTATION('',(#11215),#20163);
#20258=SHAPE_REPRESENTATION('',(#11674,#195,#196,#197,#198,#199,#200,#201,
#202),#20164);
#20259=SHAPE_REPRESENTATION('',(#11866),#20165);
#20260=SHAPE_REPRESENTATION('',(#11910,#12115,#12116,#12117,#12118,#12119,
#12120,#12121,#12122,#12123,#12124),#20166);
#20261=SHAPE_REPRESENTATION('',(#11911),#20167);
#20262=SHAPE_REPRESENTATION('',(#11956),#20168);
#20263=SHAPE_REPRESENTATION('',(#11963,#12125,#12126,#12127,#12128,#12129),
#20169);
#20264=SHAPE_REPRESENTATION('',(#11964),#20170);
#20265=SHAPE_REPRESENTATION('',(#12010),#20171);
#20266=SHAPE_REPRESENTATION('',(#12089),#20172);
#20267=SHAPE_REPRESENTATION('',(#12102),#20173);
#20268=SHAPE_REPRESENTATION('',(#12130),#20174);
#20269=SHAPE_REPRESENTATION('',(#12151),#20175);
#20270=PRODUCT_DEFINITION_CONTEXT('part definition',#20317,'design');
#20271=PRODUCT_DEFINITION('MAT-040','MAT-040',#20286,#20270);
#20272=PRODUCT_DEFINITION('Double Bracket','Double Bracket',#20287,#20270);
#20273=PRODUCT_DEFINITION('Servo Motor','Servo Motor',#20288,#20270);
#20274=PRODUCT_DEFINITION('Servo Frame','Servo Frame',#20289,#20270);
#20275=PRODUCT_DEFINITION('Gripper Link 1','Gripper Link 1',#20290,#20270);
#20276=PRODUCT_DEFINITION('Gripper Finger Assembly',
'Gripper Finger Assembly',#20291,#20270);
#20277=PRODUCT_DEFINITION('Gripper Finger','Gripper Finger',#20292,#20270);
#20278=PRODUCT_DEFINITION('Rubber Pad','Rubber Pad',#20293,#20270);
#20279=PRODUCT_DEFINITION('Gripper Bracket Assembly',
'Gripper Bracket Assembly',#20294,#20270);
#20280=PRODUCT_DEFINITION('Bearing Seat Bracket','Bearing Seat Bracket',
#20295,#20270);
#20281=PRODUCT_DEFINITION('Flanged Bearing 8x16','Flanged Bearing 8x16',
#20296,#20270);
#20282=PRODUCT_DEFINITION('Gripper Shaft 1','Gripper Shaft 1',#20297,#20270);
#20283=PRODUCT_DEFINITION('Gripper Shaft 2','Gripper Shaft 2',#20298,#20270);
#20284=PRODUCT_DEFINITION('Gripper Link 2','Gripper Link 2',#20299,#20270);
#20285=PRODUCT_DEFINITION('Socket Flat Head Screw M4x0.7x16',
'Socket Flat Head Screw M4x0.7x16',#20300,#20270);
#20286=PRODUCT_DEFINITION_FORMATION('',$,#20319);
#20287=PRODUCT_DEFINITION_FORMATION('',$,#20320);
#20288=PRODUCT_DEFINITION_FORMATION('',$,#20321);
#20289=PRODUCT_DEFINITION_FORMATION('',$,#20322);
#20290=PRODUCT_DEFINITION_FORMATION('',$,#20323);
#20291=PRODUCT_DEFINITION_FORMATION('',$,#20324);
#20292=PRODUCT_DEFINITION_FORMATION('',$,#20325);
#20293=PRODUCT_DEFINITION_FORMATION('',$,#20326);
#20294=PRODUCT_DEFINITION_FORMATION('',$,#20327);
#20295=PRODUCT_DEFINITION_FORMATION('',$,#20328);
#20296=PRODUCT_DEFINITION_FORMATION('',$,#20329);
#20297=PRODUCT_DEFINITION_FORMATION('',$,#20330);
#20298=PRODUCT_DEFINITION_FORMATION('',$,#20331);
#20299=PRODUCT_DEFINITION_FORMATION('',$,#20332);
#20300=PRODUCT_DEFINITION_FORMATION('',$,#20333);
#20301=PRODUCT_RELATED_PRODUCT_CATEGORY('MAT-040','MAT-040',(#20319));
#20302=PRODUCT_RELATED_PRODUCT_CATEGORY('Double Bracket',
'Double Bracket',(#20320));
#20303=PRODUCT_RELATED_PRODUCT_CATEGORY('Servo Motor','Servo Motor',(#20321));
#20304=PRODUCT_RELATED_PRODUCT_CATEGORY('Servo Frame','Servo Frame',(#20322));
#20305=PRODUCT_RELATED_PRODUCT_CATEGORY('Gripper Link 1',
'Gripper Link 1',(#20323));
#20306=PRODUCT_RELATED_PRODUCT_CATEGORY('Gripper Finger Assembly',
'Gripper Finger Assembly',(#20324));
#20307=PRODUCT_RELATED_PRODUCT_CATEGORY('Gripper Finger',
'Gripper Finger',(#20325));
#20308=PRODUCT_RELATED_PRODUCT_CATEGORY('Rubber Pad','Rubber Pad',(#20326));
#20309=PRODUCT_RELATED_PRODUCT_CATEGORY('Gripper Bracket Assembly',
'Gripper Bracket Assembly',(#20327));
#20310=PRODUCT_RELATED_PRODUCT_CATEGORY('Bearing Seat Bracket',
'Bearing Seat Bracket',(#20328));
#20311=PRODUCT_RELATED_PRODUCT_CATEGORY('Flanged Bearing 8x16',
'Flanged Bearing 8x16',(#20329));
#20312=PRODUCT_RELATED_PRODUCT_CATEGORY('Gripper Shaft 1',
'Gripper Shaft 1',(#20330));
#20313=PRODUCT_RELATED_PRODUCT_CATEGORY('Gripper Shaft 2',
'Gripper Shaft 2',(#20331));
#20314=PRODUCT_RELATED_PRODUCT_CATEGORY('Gripper Link 2',
'Gripper Link 2',(#20332));
#20315=PRODUCT_RELATED_PRODUCT_CATEGORY(
'Socket Flat Head Screw M4x0.7x16','Socket Flat Head Screw M4x0.7x16',(#20333));
#20316=APPLICATION_PROTOCOL_DEFINITION('international standard',
'automotive_design',2009,#20317);
#20317=APPLICATION_CONTEXT(
'Core Data for Automotive Mechanical Design Process');
#20318=PRODUCT_CONTEXT('part definition',#20317,'mechanical');
#20319=PRODUCT('MAT-040','MAT-040','STEP AP214',(#20318));
#20320=PRODUCT('Double Bracket','Double Bracket',$,(#20318));
#20321=PRODUCT('Servo Motor','Servo Motor',$,(#20318));
#20322=PRODUCT('Servo Frame','Servo Frame',$,(#20318));
#20323=PRODUCT('Gripper Link 1','Gripper Link 1',$,(#20318));
#20324=PRODUCT('Gripper Finger Assembly','Gripper Finger Assembly',$,(#20318));
#20325=PRODUCT('Gripper Finger','Gripper Finger',$,(#20318));
#20326=PRODUCT('Rubber Pad','Rubber Pad',$,(#20318));
#20327=PRODUCT('Gripper Bracket Assembly','Gripper Bracket Assembly',$,
(#20318));
#20328=PRODUCT('Bearing Seat Bracket','Bearing Seat Bracket',$,(#20318));
#20329=PRODUCT('Flanged Bearing 8x16','Flanged Bearing 8x16',$,(#20318));
#20330=PRODUCT('Gripper Shaft 1','Gripper Shaft 1',$,(#20318));
#20331=PRODUCT('Gripper Shaft 2','Gripper Shaft 2',$,(#20318));
#20332=PRODUCT('Gripper Link 2','Gripper Link 2',$,(#20318));
#20333=PRODUCT('Socket Flat Head Screw M4x0.7x16',
'Socket Flat Head Screw M4x0.7x16',$,(#20318));
#20334=PRESENTATION_STYLE_ASSIGNMENT((#20339));
#20335=PRESENTATION_STYLE_ASSIGNMENT((#20340));
#20336=PRESENTATION_STYLE_ASSIGNMENT((#20341));
#20337=PRESENTATION_STYLE_ASSIGNMENT((#20342));
#20338=PRESENTATION_STYLE_ASSIGNMENT((#20343));
#20339=SURFACE_STYLE_USAGE(.BOTH.,#20344);
#20340=SURFACE_STYLE_USAGE(.BOTH.,#20345);
#20341=SURFACE_STYLE_USAGE(.BOTH.,#20346);
#20342=SURFACE_STYLE_USAGE(.BOTH.,#20347);
#20343=SURFACE_STYLE_USAGE(.BOTH.,#20348);
#20344=SURFACE_SIDE_STYLE('',(#20349));
#20345=SURFACE_SIDE_STYLE('',(#20350));
#20346=SURFACE_SIDE_STYLE('',(#20351));
#20347=SURFACE_SIDE_STYLE('',(#20352));
#20348=SURFACE_SIDE_STYLE('',(#20353));
#20349=SURFACE_STYLE_FILL_AREA(#20354);
#20350=SURFACE_STYLE_FILL_AREA(#20355);
#20351=SURFACE_STYLE_FILL_AREA(#20356);
#20352=SURFACE_STYLE_FILL_AREA(#20357);
#20353=SURFACE_STYLE_FILL_AREA(#20358);
#20354=FILL_AREA_STYLE('Steel - Satin',(#20359));
#20355=FILL_AREA_STYLE('Opaque(20,51,87)',(#20360));
#20356=FILL_AREA_STYLE('Opaque(97,158,199)',(#20361));
#20357=FILL_AREA_STYLE('Opaque(31,36,43)',(#20362));
#20358=FILL_AREA_STYLE('Opaque(122,133,145)',(#20363));
#20359=FILL_AREA_STYLE_COLOUR('Steel - Satin',#20364);
#20360=FILL_AREA_STYLE_COLOUR('Opaque(20,51,87)',#20365);
#20361=FILL_AREA_STYLE_COLOUR('Opaque(97,158,199)',#20366);
#20362=FILL_AREA_STYLE_COLOUR('Opaque(31,36,43)',#20367);
#20363=FILL_AREA_STYLE_COLOUR('Opaque(122,133,145)',#20368);
#20364=COLOUR_RGB('Steel - Satin',0.627450980392157,0.627450980392157,0.627450980392157);
#20365=COLOUR_RGB('Opaque(20,51,87)',0.0784313725490196,0.2,0.341176470588235);
#20366=COLOUR_RGB('Opaque(97,158,199)',0.380392156862745,0.619607843137255,
0.780392156862745);
#20367=COLOUR_RGB('Opaque(31,36,43)',0.12156862745098,0.141176470588235,
0.168627450980392);
#20368=COLOUR_RGB('Opaque(122,133,145)',0.47843137254902,0.52156862745098,
0.568627450980392);
ENDSEC;
END-ISO-10303-21;
